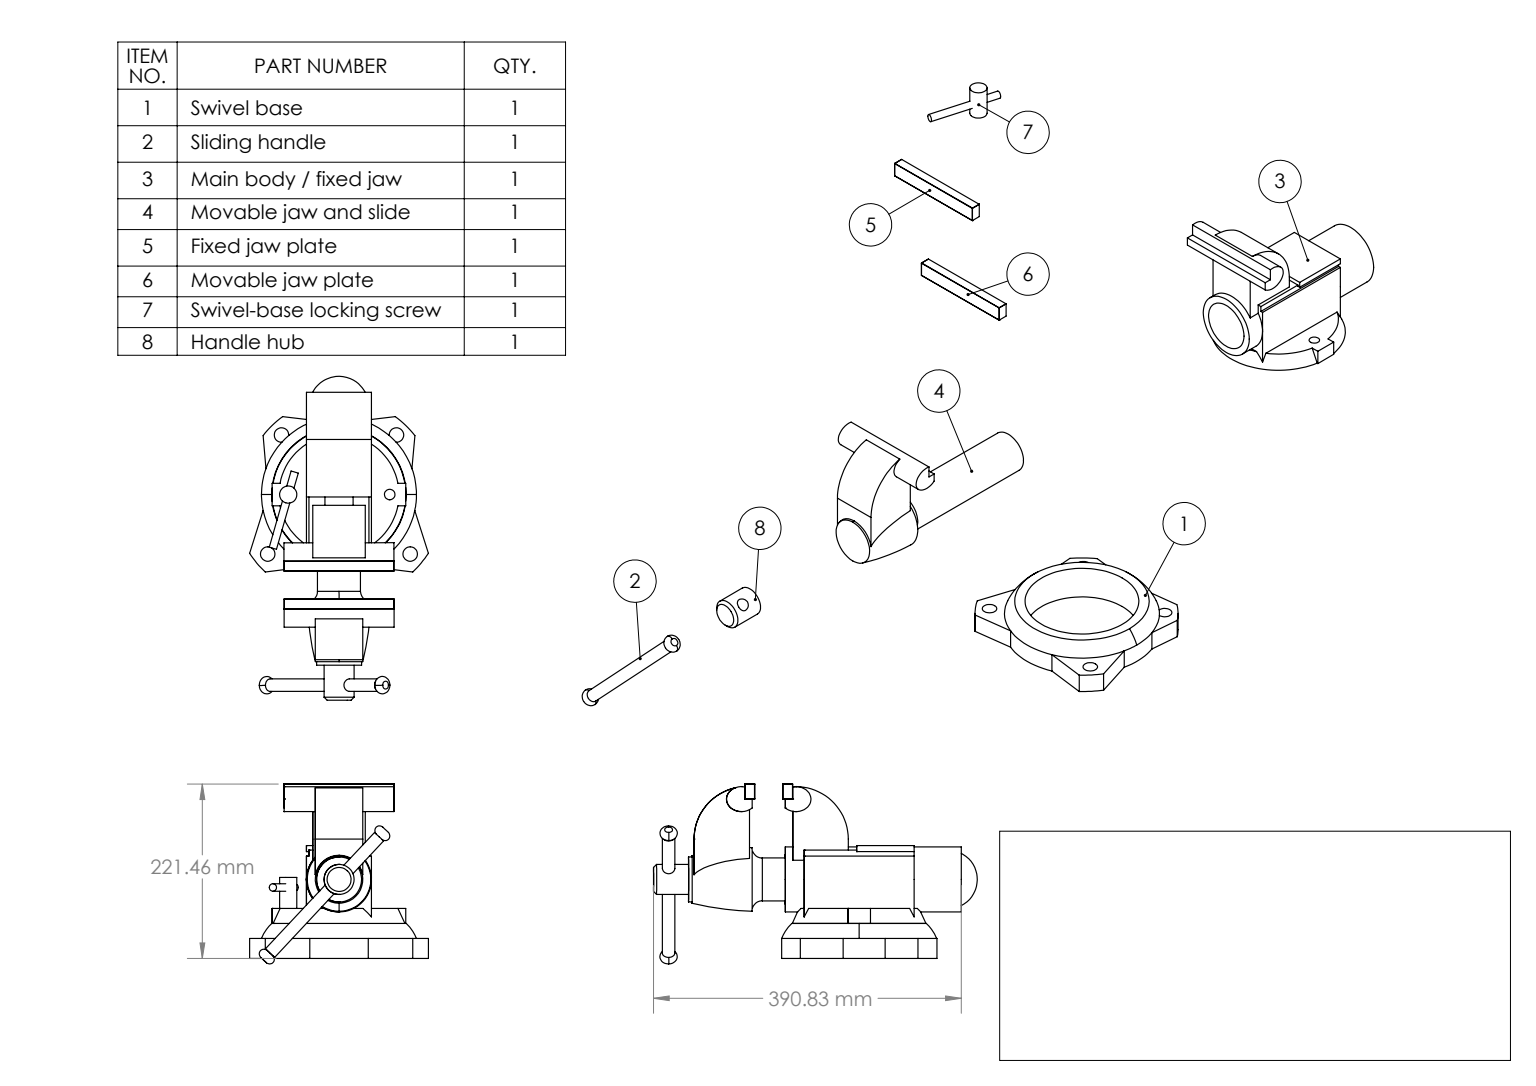
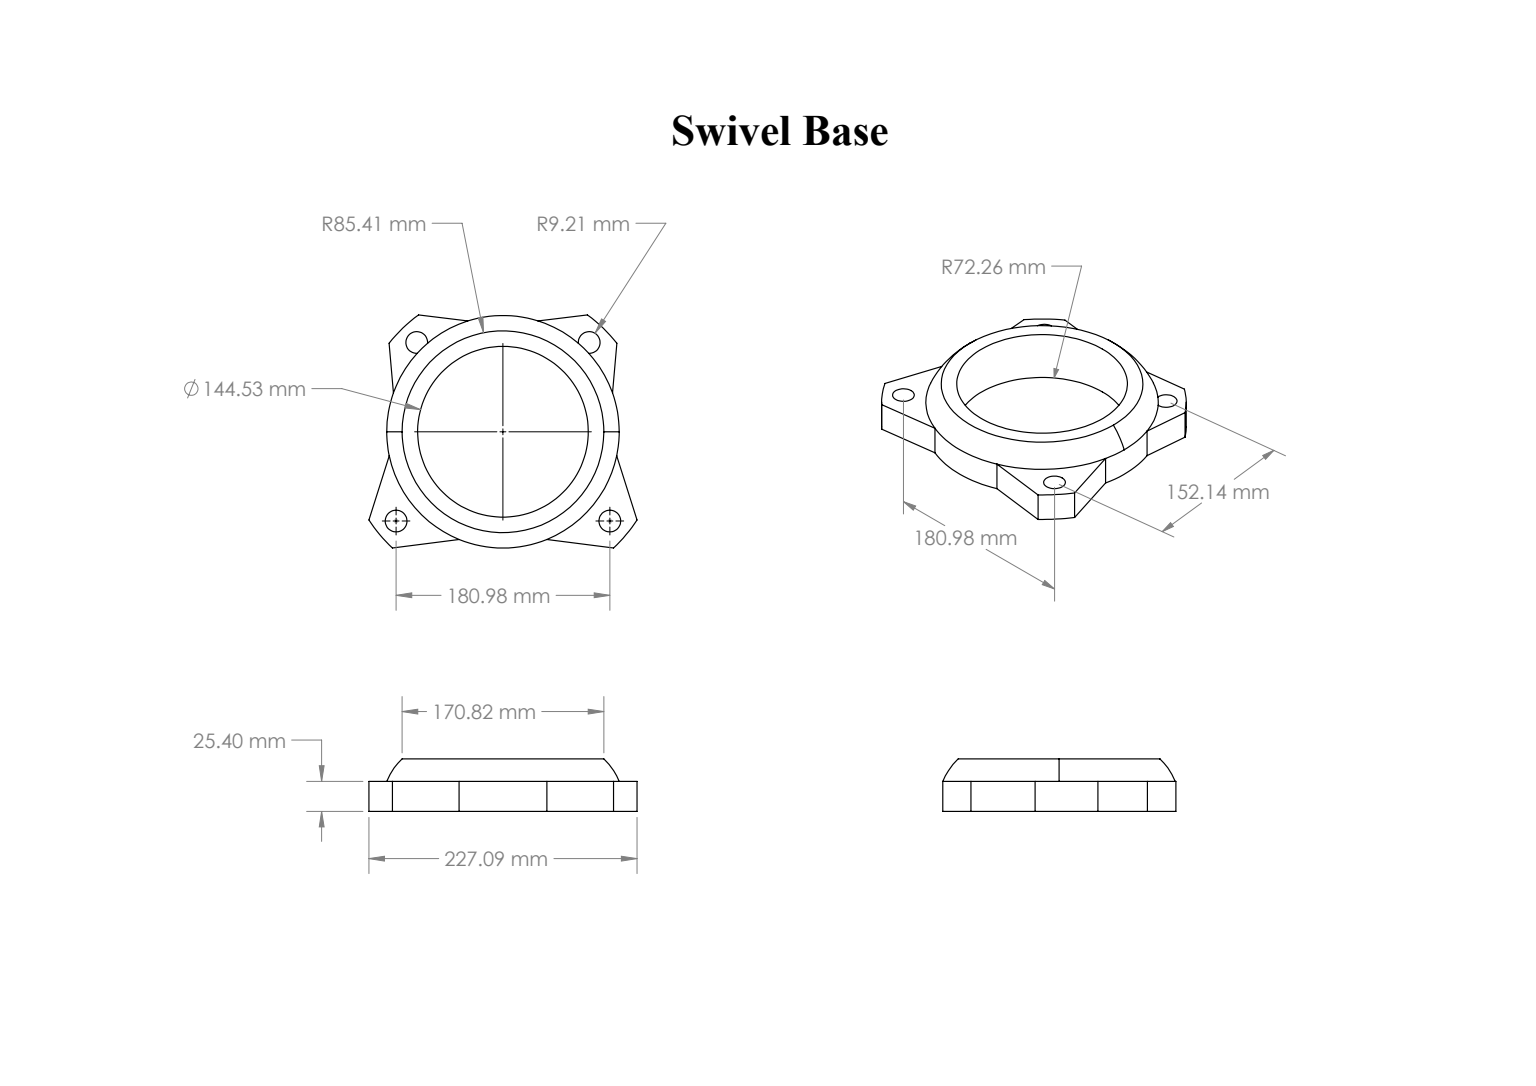
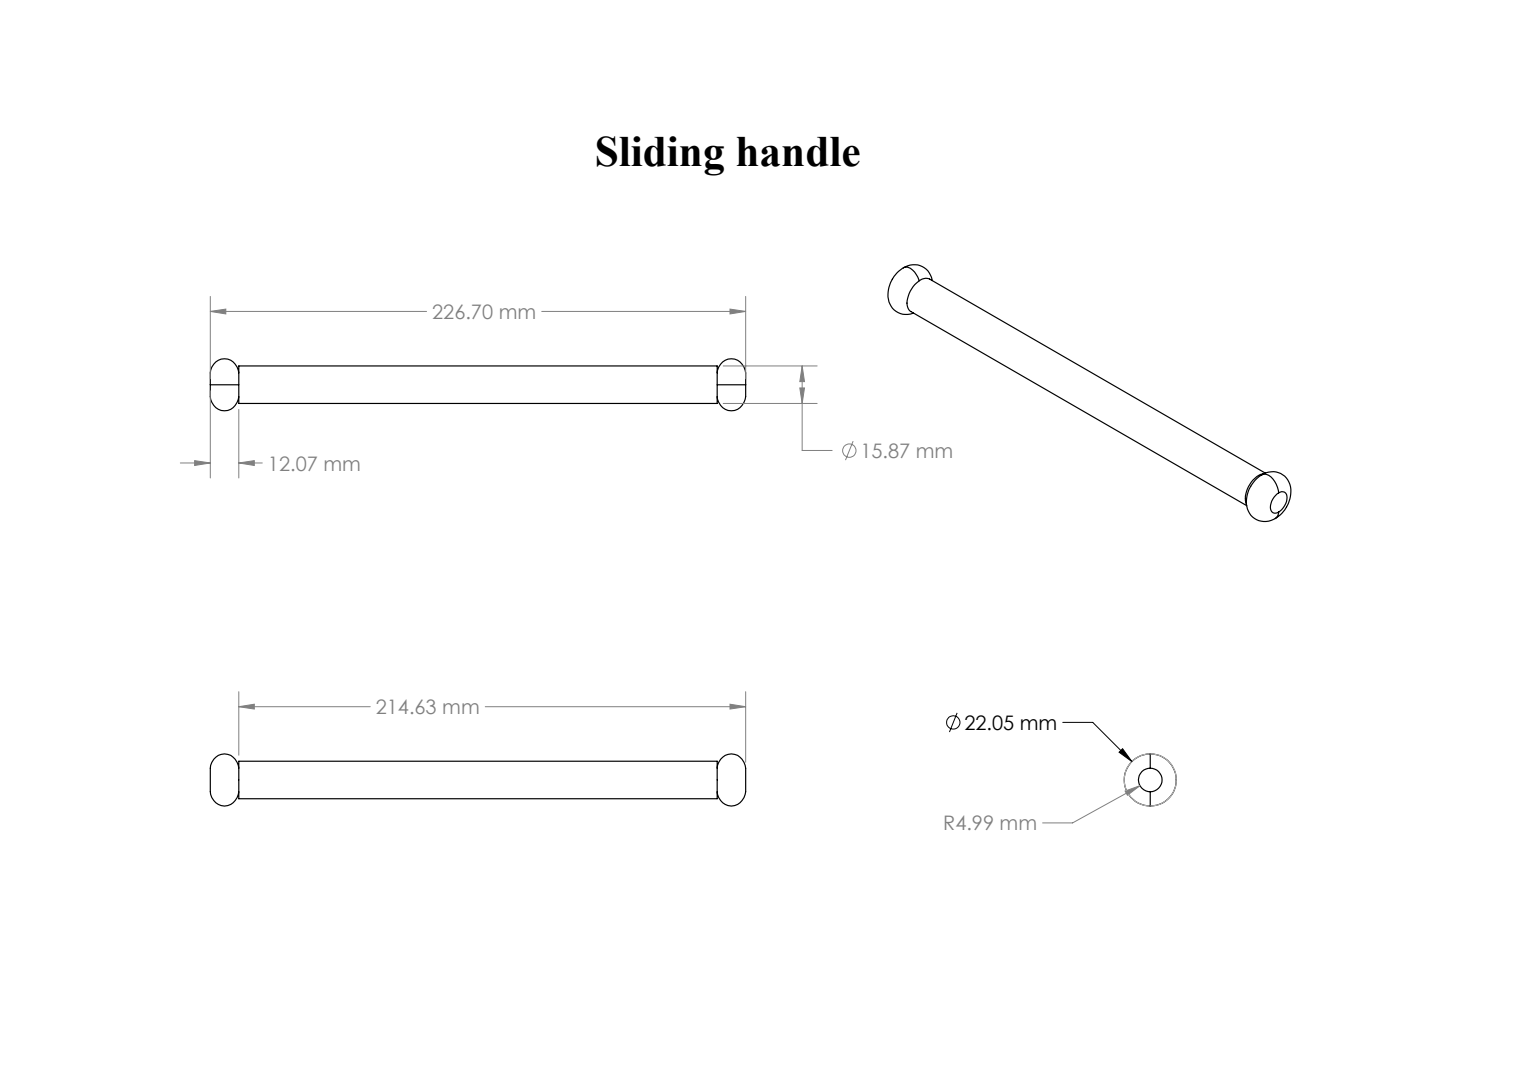
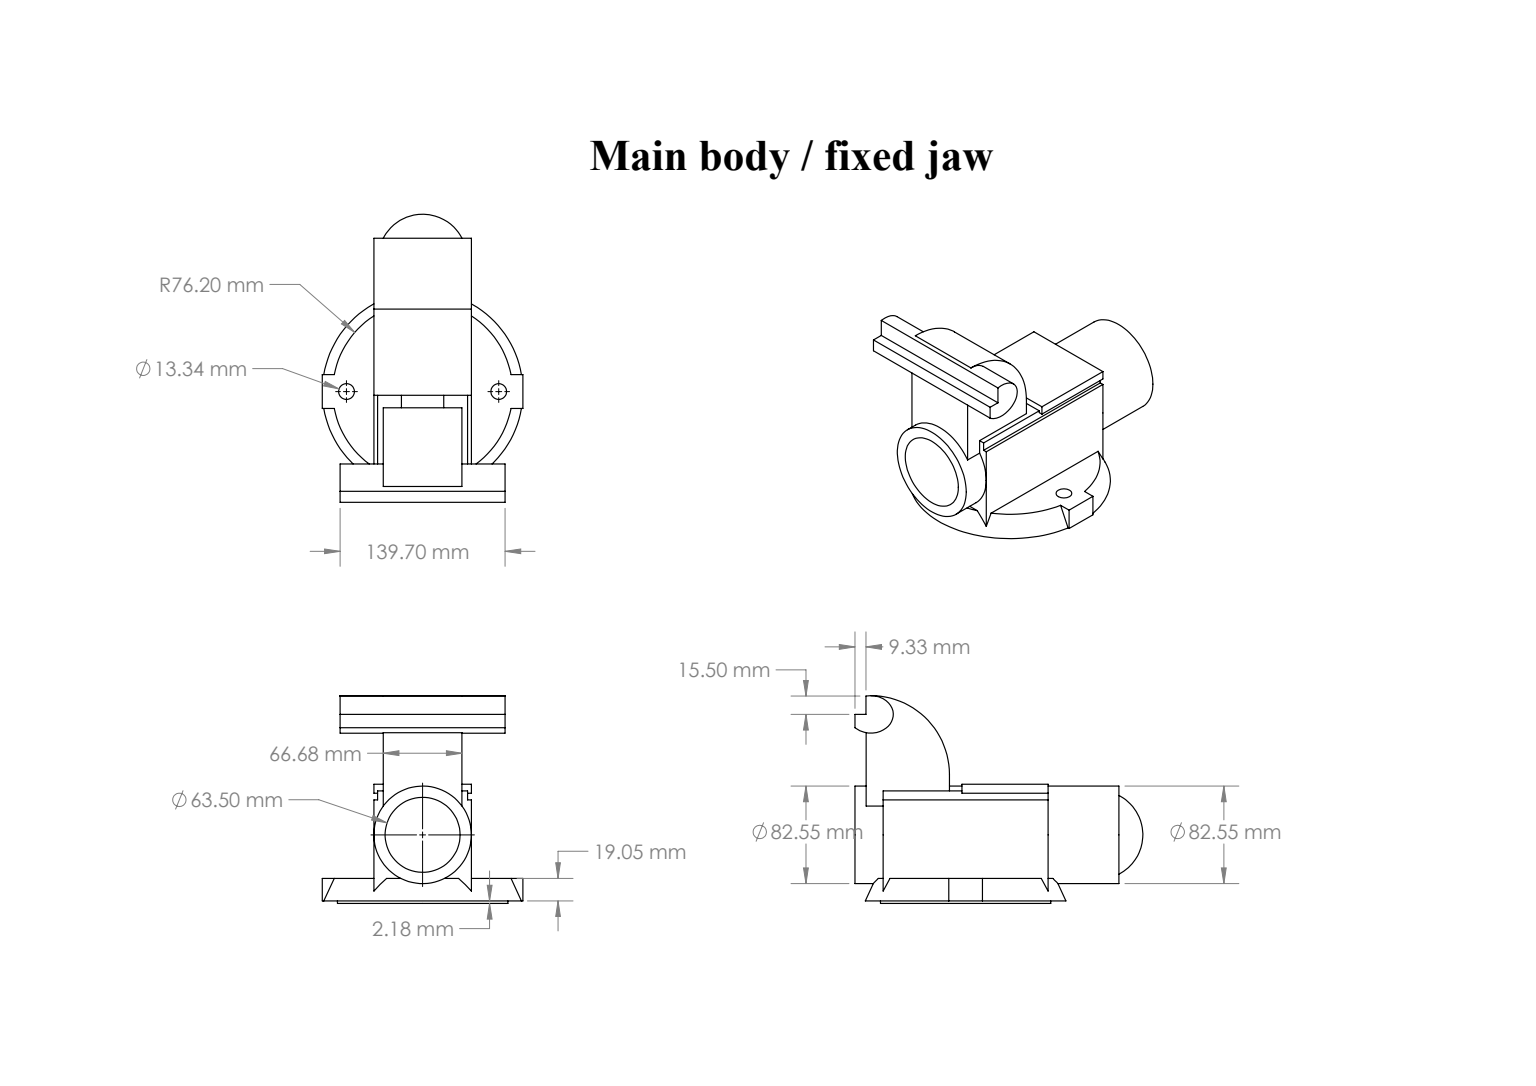
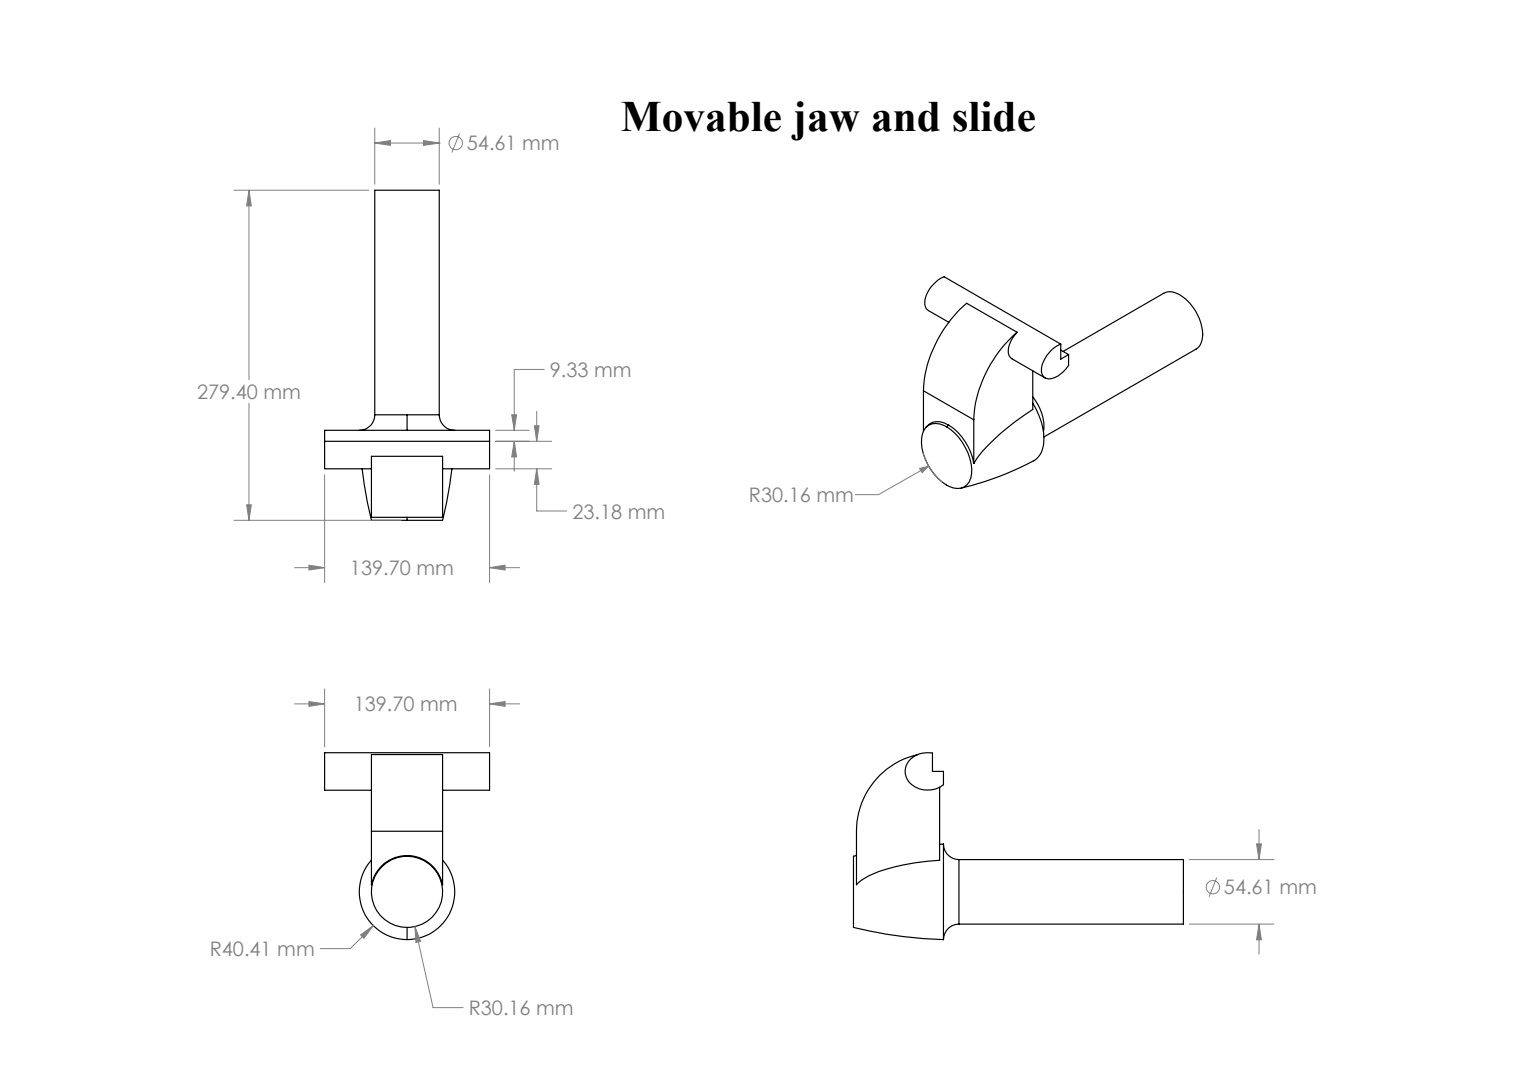
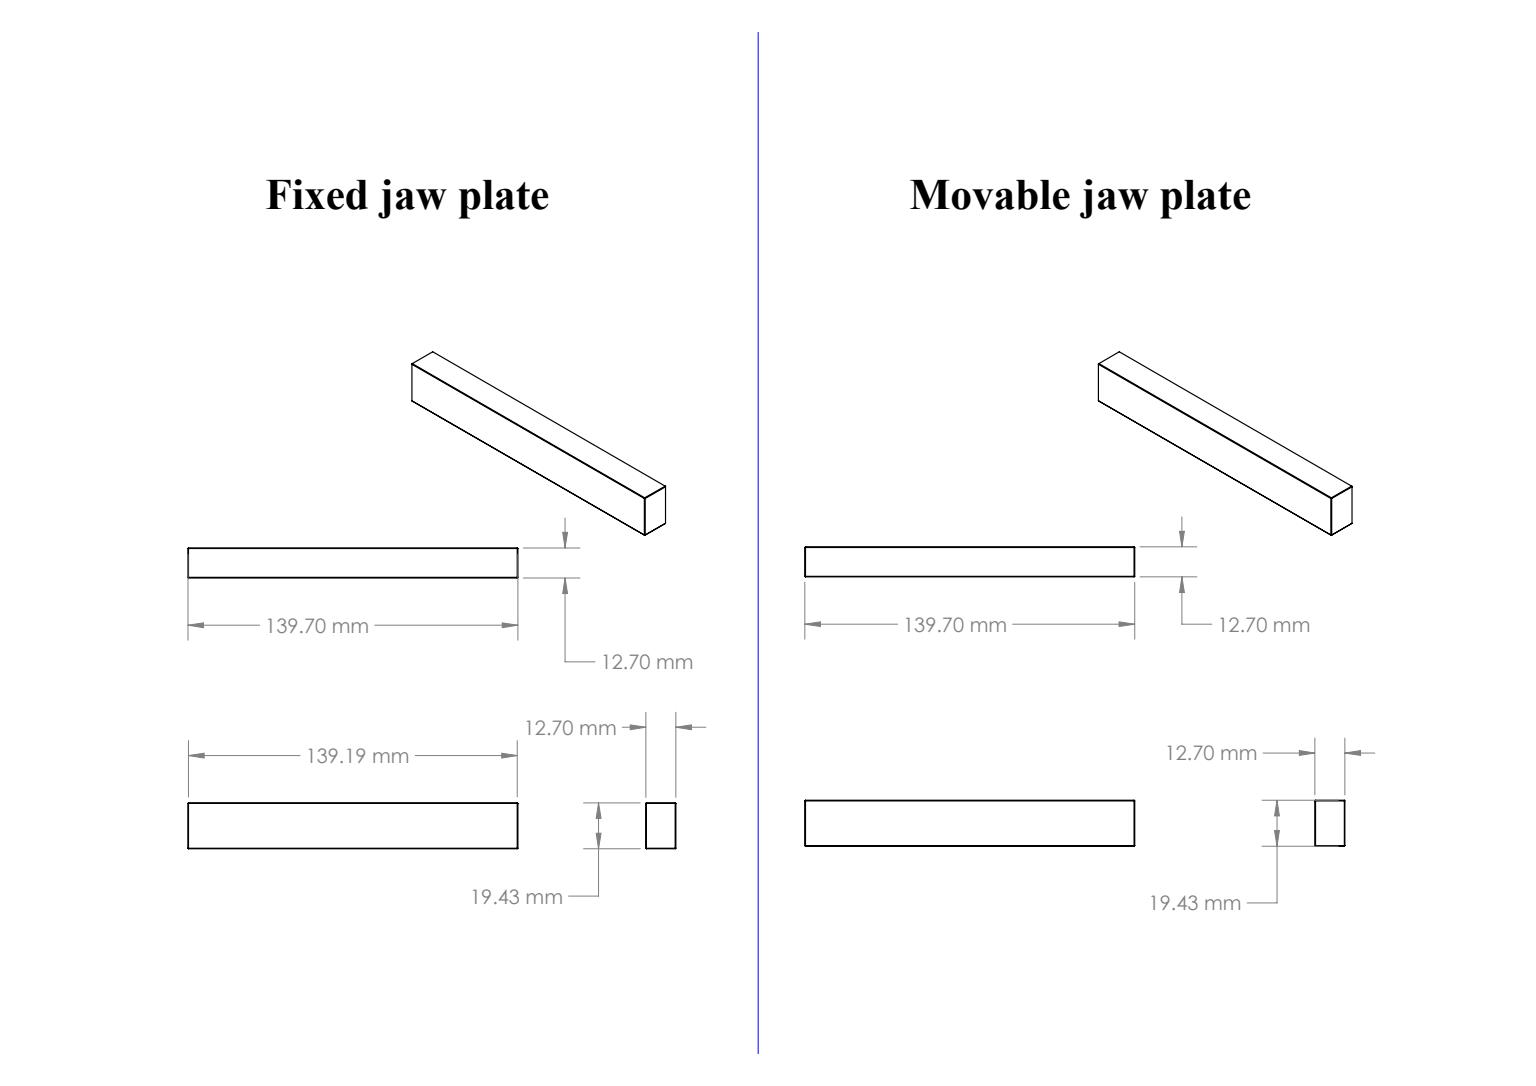
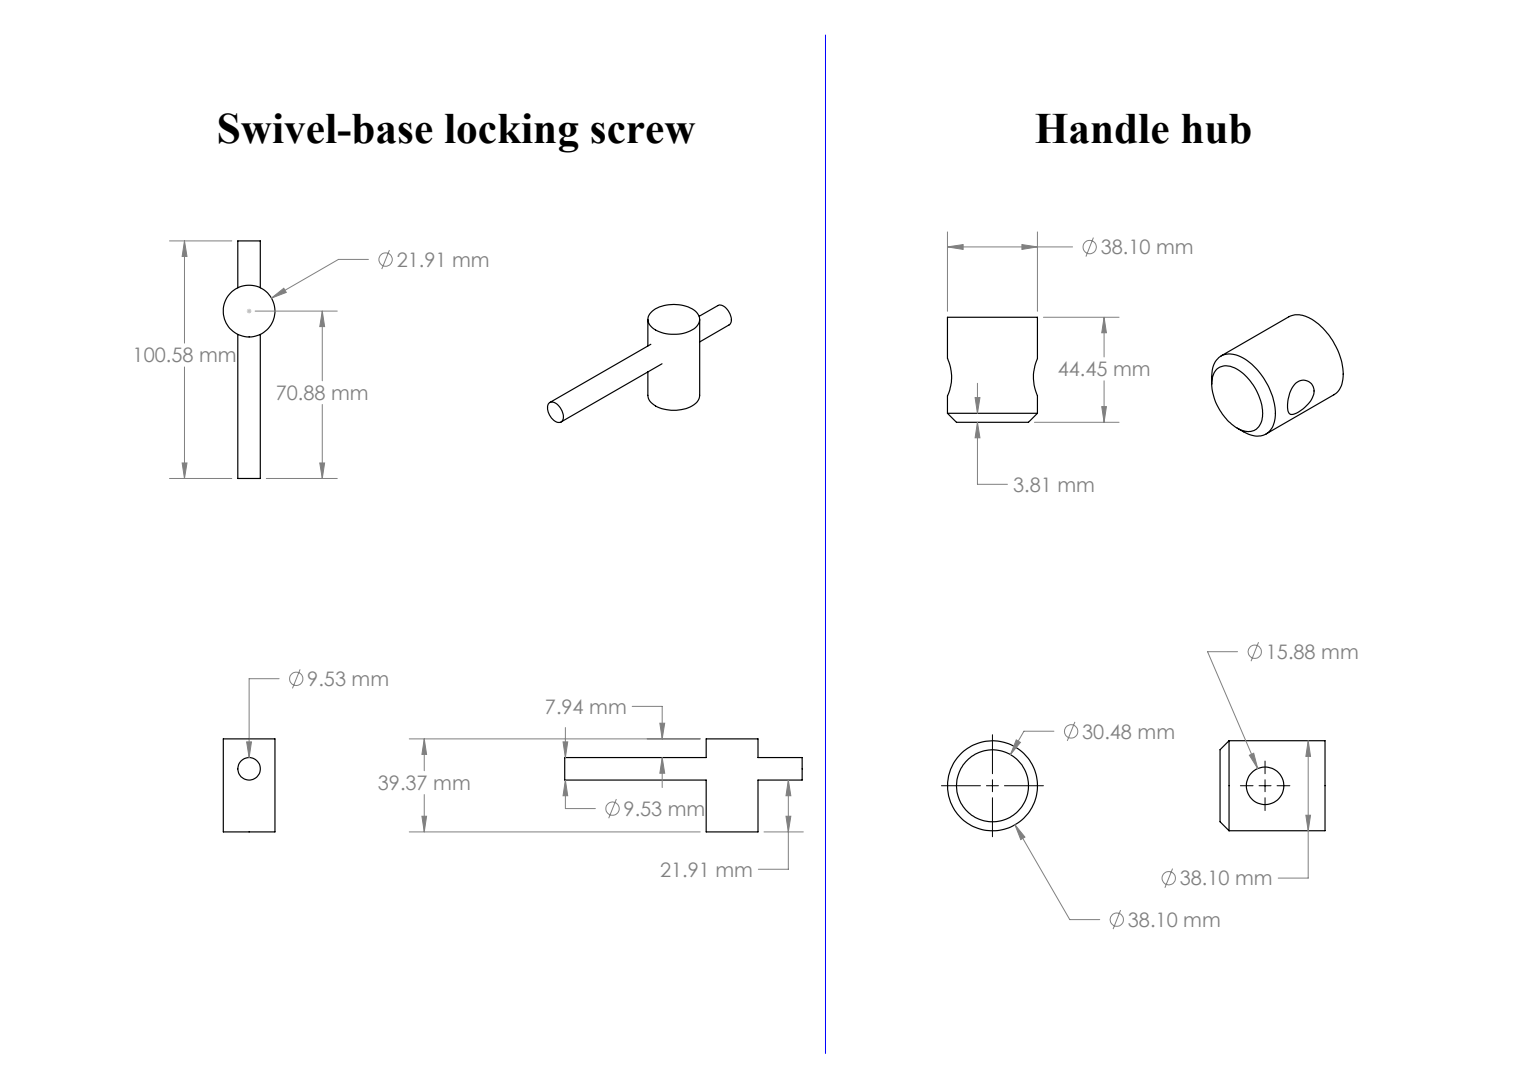
ISO-10303-21;
HEADER;
FILE_DESCRIPTION (('STEP AP203'),
    '1' );
FILE_NAME ('MAS-412',
    '2026-10-07T23:37:23',
    ( '' ),
    ( '' ),
    'SwSTEP 2.0',
    'SolidWorks 2024',
    '' );
FILE_SCHEMA (( 'AUTOMOTIVE_DESIGN' ));
ENDSEC;

DATA;
#1 = EDGE_CURVE ( 'NONE', #6151, #2183, #1599, .T. ) ;
#2 = DIRECTION ( 'NONE',  ( 1.000000000000000000, 0.000000000000000000, 0.000000000000000000 ) ) ;
#3 = CARTESIAN_POINT ( 'NONE',  ( 2.750000000000000444, 8.719000000000002970, 4.313750000000002416 ) ) ;
#4 = CARTESIAN_POINT ( 'NONE',  ( 2.740000000000000213, 8.729000000000002757, 3.333750000000001990 ) ) ;
#5 = ORIENTED_EDGE ( 'NONE', *, *, #5735, .T. ) ;
#6 = CALENDAR_DATE ( 2026, 8, 10 ) ;
#7 = CARTESIAN_POINT ( 'NONE',  ( 2.537500000000000533, 2.500000000000000444, 0.2625000000000008438 ) ) ;
#8 = ADVANCED_FACE ( 'NONE', ( #7344 ), #2858, .F. ) ;
#9 = CARTESIAN_POINT ( 'NONE',  ( -8.751021560936518753E-10, 1.365923996832131609E-16, 5.750408897959578548E-10 ) ) ;
#10 = COORDINATED_UNIVERSAL_TIME_OFFSET ( 0, 0, .AHEAD. ) ;
#11 = CARTESIAN_POINT ( 'NONE',  ( -0.7335700379171464780, 2.500000000182677873, -2.908930215554831999 ) ) ;
#12 = PLANE ( 'NONE',  #8081 ) ;
#13 = ADVANCED_FACE ( 'NONE', ( #7172 ), #6014, .F. ) ;
#14 = AXIS2_PLACEMENT_3D ( 'NONE', #1376, #7034, #673 ) ;
#15 = CYLINDRICAL_SURFACE ( 'NONE', #5940, 2.841000000000000636 ) ;
#16 = CARTESIAN_POINT ( 'NONE',  ( 3.544128228010244186, 1.000000000000000000, 1.972857804739797549 ) ) ;
#17 = ORIENTED_EDGE ( 'NONE', *, *, #5224, .F. ) ;
#18 = LINE ( 'NONE', #3837, #1501 ) ;
#19 = EDGE_CURVE ( 'NONE', #3352, #6547, #5345, .T. ) ;
#20 = CARTESIAN_POINT ( 'NONE',  ( -1.187499999999999778, 4.475358323637860458, 6.462174474937253166 ) ) ;
#21 = APPROVAL_DATE_TIME ( #5612, #98 ) ;
#22 = ORIENTED_EDGE ( 'NONE', *, *, #441, .F. ) ;
#23 = DIRECTION ( 'NONE',  ( 0.000000000000000000, 0.000000000000000000, 1.000000000000000000 ) ) ;
#24 = AXIS2_PLACEMENT_3D ( 'NONE', #1125, #5495, #3538 ) ;
#25 = VECTOR ( 'NONE', #5396, 39.37007874015748143 ) ;
#26 = DIRECTION ( 'NONE',  ( -0.000000000000000000, -1.000000000000000000, -0.000000000000000000 ) ) ;
#27 = LINE ( 'NONE', #5041, #2456 ) ;
#28 = AXIS2_PLACEMENT_3D ( 'NONE', #2617, #7646, #6878 ) ;
#29 = CARTESIAN_POINT ( 'NONE',  ( -2.750000000000000444, 8.601289606299213020, 5.246732086614174229 ) ) ;
#30 = ORIENTED_EDGE ( 'NONE', *, *, #1937, .F. ) ;
#31 = EDGE_LOOP ( 'NONE', ( #4317, #4718, #4653 ) ) ;
#32 = AXIS2_PLACEMENT_3D ( 'NONE', #473, #3002, #4187 ) ;
#33 =( BOUNDED_SURFACE ( )  B_SPLINE_SURFACE ( 3, 3, ( 
 ( #3117, #4870, #7402, #4254 ),
 ( #5609, #6767, #8175, #1152 ),
 ( #198, #3878, #2545, #7053 ),
 ( #4418, #1438, #7009, #3230 ),
 ( #1275, #1924, #4991, #5814 ),
 ( #6924, #3192, #7610, #6392 ) ),
 .UNSPECIFIED., .F., .F., .F. ) 
 B_SPLINE_SURFACE_WITH_KNOTS ( ( 4, 2, 4 ),
 ( 4, 4 ),
 ( 0.000000000000000000, 0.5000000000000000000, 1.000000000000000000 ),
 ( 0.000000000000000000, 1.000000000000000000 ),
 .UNSPECIFIED. ) 
 GEOMETRIC_REPRESENTATION_ITEM ( )  RATIONAL_B_SPLINE_SURFACE ( (
 ( 1.000000000000000000, 0.3333333333333334259, 0.3333333333333334259, 1.000000000000000000),
 ( 1.000000000000000000, 0.3333333333333334259, 0.3333333333333334259, 1.000000000000000000),
 ( 1.000000000000000000, 0.3333333333333334259, 0.3333333333333334259, 1.000000000000000000),
 ( 1.000000000000000000, 0.3333333333333334259, 0.3333333333333334259, 1.000000000000000000),
 ( 1.000000000000000000, 0.3333333333333334259, 0.3333333333333334259, 1.000000000000000000),
 ( 1.000000000000000000, 0.3333333333333334259, 0.3333333333333334259, 1.000000000000000000) ) ) 
 REPRESENTATION_ITEM ( '' )  SURFACE ( )  );
#34 = AXIS2_PLACEMENT_3D ( 'NONE', #7877, #946, #1033 ) ;
#35 = APPROVAL_PERSON_ORGANIZATION ( #57, #5208, #4410 ) ;
#36 = ADVANCED_FACE ( 'NONE', ( #6211 ), #602, .T. ) ;
#37 = CARTESIAN_POINT ( 'NONE',  ( -0.5082965702588324586, 2.405310912759768716, -3.001266468626919259 ) ) ;
#38 = CARTESIAN_POINT ( 'NONE',  ( 0.8670765961576291092, 4.936241069566050577, -5.108749999999999680 ) ) ;
#39 = AXIS2_PLACEMENT_3D ( 'NONE', #7359, #1153, #8008 ) ;
#40 = DIRECTION ( 'NONE',  ( -1.000000000000000000, 0.000000000000000000, 0.000000000000000000 ) ) ;
#41 = VERTEX_POINT ( 'NONE', #2074 ) ;
#42 = ADVANCED_FACE ( 'NONE', ( #1382 ), #6295, .T. ) ;
#43 = DATE_AND_TIME ( #3168, #965 ) ;
#44 = AXIS2_PLACEMENT_3D ( 'NONE', #2089, #4037, #244 ) ;
#45 = CARTESIAN_POINT ( 'NONE',  ( 3.987953385826772390, 3.755224612465394962, 8.262149156879575074 ) ) ;
#46 = CARTESIAN_POINT ( 'NONE',  ( -0.7335374419612978869, 3.792759758930658531, 8.502074107329825381 ) ) ;
#47 = VERTEX_POINT ( 'NONE', #5759 ) ;
#48 = AXIS2_PLACEMENT_3D ( 'NONE', #4004, #7908, #4660 ) ;
#49 = CC_DESIGN_PERSON_AND_ORGANIZATION_ASSIGNMENT ( #5339, #2324, ( #1030 ) ) ;
#50 =( GEOMETRIC_REPRESENTATION_CONTEXT ( 3 ) GLOBAL_UNCERTAINTY_ASSIGNED_CONTEXT ( ( #4134 ) ) GLOBAL_UNIT_ASSIGNED_CONTEXT ( ( #3153, #3070, #7613 ) ) REPRESENTATION_CONTEXT ( 'NONE', 'WORKASPACE' ) );
#51 = FACE_BOUND ( 'NONE', #4197, .T. ) ;
#52 = CARTESIAN_POINT ( 'NONE',  ( 4.462953385826772035, 3.753500037802128375, 8.231249998505111520 ) ) ;
#53 = PLANE ( 'NONE',  #82 ) ;
#54 = ORIENTED_EDGE ( 'NONE', *, *, #6929, .T. ) ;
#55 = APPROVAL_DATE_TIME ( #6339, #5621 ) ;
#56 = CARTESIAN_POINT ( 'NONE',  ( 2.750000000000000444, 8.601278779527561369, 5.246694173228347857 ) ) ;
#57 = PERSON_AND_ORGANIZATION ( #1568, #5834 ) ;
#58 = CARTESIAN_POINT ( 'NONE',  ( -2.740000000000001545, 7.973999999999999311, 4.323750000000001315 ) ) ;
#59 = CARTESIAN_POINT ( 'NONE',  ( 1.625000000000000222, 5.113999999999999879, -2.750000000000000444 ) ) ;
#60 = APPROVAL_PERSON_ORGANIZATION ( #7787, #6874, #5361 ) ;
#61 = ADVANCED_FACE ( 'NONE', ( #5673, #1333, #92, #2030, #51, #5721 ), #132, .F. ) ;
#62 = EDGE_CURVE ( 'NONE', #2284, #7136, #4477, .T. ) ;
#63 = CARTESIAN_POINT ( 'NONE',  ( -3.987046614173229919, 3.872296061808612411, 8.050752829671743882 ) ) ;
#64 = AXIS2_PLACEMENT_3D ( 'NONE', #1983, #3374, #5790 ) ;
#65 = ORIENTED_EDGE ( 'NONE', *, *, #1296, .T. ) ;
#66 = DIRECTION ( 'NONE',  ( 2.664535259084986204E-15, 0.000000000000000000, 1.000000000000000000 ) ) ;
#67 = DIRECTION ( 'NONE',  ( 0.000000000000000000, 0.000000000000000000, 1.000000000000000000 ) ) ;
#68 = CARTESIAN_POINT ( 'NONE',  ( -1.187500000000000000, 4.528589268181947070, 6.350981843454763798 ) ) ;
#69 = DATE_AND_TIME ( #5694, #2477 ) ;
#70 = EDGE_LOOP ( 'NONE', ( #2555, #6227 ) ) ;
#71 = FACE_OUTER_BOUND ( 'NONE', #866, .T. ) ;
#72 = AXIS2_PLACEMENT_3D ( 'NONE', #6327, #85, #2600 ) ;
#73 = CIRCLE ( 'NONE', #872, 1.124999999999999556 ) ;
#74 = CARTESIAN_POINT ( 'NONE',  ( -4.462046614173229564, 3.753500037802127043, 8.231249998505111520 ) ) ;
#75 = VECTOR ( 'NONE', #6916, 39.37007874015748854 ) ;
#76 = PLANE ( 'NONE',  #326 ) ;
#77 = CARTESIAN_POINT ( 'NONE',  ( 0.000000000000000000, 3.950000000000000178, 2.749999999536766992 ) ) ;
#78 = EDGE_CURVE ( 'NONE', #6387, #3627, #5164, .T. ) ;
#79 = EDGE_CURVE ( 'NONE', #5487, #520, #4524, .T. ) ;
#80 = ORIENTED_EDGE ( 'NONE', *, *, #6042, .T. ) ;
#81 = ORIENTED_EDGE ( 'NONE', *, *, #8030, .T. ) ;
#82 = AXIS2_PLACEMENT_3D ( 'NONE', #2571, #5061, #7600 ) ;
#83 = DIRECTION ( 'NONE',  ( 1.000000000000000000, 0.000000000000000000, 0.000000000000000000 ) ) ;
#84 = CARTESIAN_POINT ( 'NONE',  ( -0.001186137648316157355, 2.637500537863615158, -5.108750000000001457 ) ) ;
#85 = DIRECTION ( 'NONE',  ( -1.000000000000000000, 0.000000000000000000, 0.000000000000000000 ) ) ;
#86 = ORIENTED_EDGE ( 'NONE', *, *, #479, .F. ) ;
#87 = CARTESIAN_POINT ( 'NONE',  ( 3.987953385826771946, 3.763524128032369465, 8.293365503768654889 ) ) ;
#88 = DIMENSIONAL_EXPONENTS ( 1.000000000000000000, 0.000000000000000000, 0.000000000000000000, 0.000000000000000000, 0.000000000000000000, 0.000000000000000000, 0.000000000000000000 ) ;
#89 = DIRECTION ( 'NONE',  ( 0.9917930140014037388, -0.000000000000000000, 0.1278538907425633420 ) ) ;
#90 = ORIENTED_EDGE ( 'NONE', *, *, #3285, .F. ) ;
#91 = CARTESIAN_POINT ( 'NONE',  ( 0.000000000000000000, 3.950000000000000178, -5.108750000000001457 ) ) ;
#92 = FACE_BOUND ( 'NONE', #7637, .T. ) ;
#93 = DIRECTION ( 'NONE',  ( 0.7071067811865474617, -0.7071067811865474617, -0.000000000000000000 ) ) ;
#94 =( REPRESENTATION_RELATIONSHIP ('NONE','NONE', #3256, #4813 ) REPRESENTATION_RELATIONSHIP_WITH_TRANSFORMATION ( #6716 )SHAPE_REPRESENTATION_RELATIONSHIP( ) );
#95 = VERTEX_POINT ( 'NONE', #3821 ) ;
#96 = SHAPE_DEFINITION_REPRESENTATION ( #1706, #2780 ) ;
#97 = LINE ( 'NONE', #5064, #3478 ) ;
#98 = APPROVAL ( #5739, 'UNSPECIFIED' ) ;
#99 = CARTESIAN_POINT ( 'NONE',  ( -1.489119986720869093, 2.223645902163796428, 2.750000000000000444 ) ) ;
#100 = PRODUCT_DEFINITION_SHAPE ( 'NONE', 'NONE',  #1914 ) ;
#101 = EDGE_LOOP ( 'NONE', ( #3409, #718, #7066 ) ) ;
#102 = ADVANCED_FACE ( 'NONE', ( #760 ), #2649, .T. ) ;
#103 = CARTESIAN_POINT ( 'NONE',  ( 0.000000000000000000, 1.664000000000000368, 2.693920355039552791E-42 ) ) ;
#104 = CARTESIAN_POINT ( 'NONE',  ( 1.312500000000000444, 8.589000000000002188, 3.161250000147724837 ) ) ;
#105 = CARTESIAN_POINT ( 'NONE',  ( -3.987046614173230363, 4.023873226579398832, 8.413336896757355632 ) ) ;
#106 = ORIENTED_EDGE ( 'NONE', *, *, #5767, .F. ) ;
#107 = CARTESIAN_POINT ( 'NONE',  ( -8.751021560936518753E-10, 1.365923996832131609E-16, 5.750408897959578548E-10 ) ) ;
#108 = CARTESIAN_POINT ( 'NONE',  ( 2.750000000000000444, 8.574153543307087233, 4.323749999999999538 ) ) ;
#109 = B_SPLINE_CURVE_WITH_KNOTS ( 'NONE', 3,
 ( #7082, #3263, #3389, #1429, #5254, #2158, #2655, #2036, #5139, #5854, #6561, #3992, #235, #929, #7685, #3940, #3903, #2080, #4572, #1464, #6222, #3185, #4487, #140, #5807, #5908, #7147, #1492, #3971, #260, #7791, #6408, #825, #7023, #3369, #6543, #3328, #1535, #1412, #2138, #7710, #954, #5832, #214 ),
 .UNSPECIFIED., .F., .F.,
 ( 4, 2, 2, 2, 2, 2, 2, 2, 2, 2, 2, 2, 2, 2, 2, 2, 2, 2, 2, 2, 2, 4 ),
 ( 1.387778780781445676E-17, 0.001568404162335165731, 0.002352606243502761499, 0.003136808324670357917, 0.004705212487005582846, 0.005489414568173214826, 0.006273616649340845071, 0.007842020811676163675, 0.009410424974011483146, 0.01019462705517914375, 0.01097882913634680262, 0.01254723329868211515, 0.01333143537984972891, 0.01411563746101734441, 0.01568404162335264307, 0.01725244578568794346, 0.01882084994802324038, 0.02038925411035854424, 0.02117345619152621525, 0.02195765827269388973, 0.02352606243502923522, 0.02509446659736457724 ),
 .UNSPECIFIED. ) ;
#110 = COORDINATED_UNIVERSAL_TIME_OFFSET ( 0, 0, .AHEAD. ) ;
#111 = ORIENTED_EDGE ( 'NONE', *, *, #1410, .F. ) ;
#112 = CARTESIAN_POINT ( 'NONE',  ( -2.750000000000000444, 8.601278779527561369, 3.691250000000001030 ) ) ;
#113 = EDGE_CURVE ( 'NONE', #6547, #6766, #6910, .T. ) ;
#114 = FACE_OUTER_BOUND ( 'NONE', #4631, .T. ) ;
#115 = DIRECTION ( 'NONE',  ( 0.000000000000000000, -1.000000000000000000, -0.000000000000000000 ) ) ;
#116 = PLANE ( 'NONE',  #837 ) ;
#117 = ORIENTED_EDGE ( 'NONE', *, *, #7488, .F. ) ;
#118 = ADVANCED_FACE ( 'NONE', ( #182 ), #7038, .F. ) ;
#119 = ORIENTED_EDGE ( 'NONE', *, *, #2557, .F. ) ;
#120 = APPROVAL_PERSON_ORGANIZATION ( #3902, #1264, #2035 ) ;
#121 = DIRECTION ( 'NONE',  ( 0.000000000000000000, -1.000000000000000000, 0.000000000000000000 ) ) ;
#122 = CARTESIAN_POINT ( 'NONE',  ( 1.282759084805754402, 3.671339687942380525, -5.108750000000001457 ) ) ;
#123 = CARTESIAN_POINT ( 'NONE',  ( 0.7335700383277801162, 2.500000000390421473, -2.908930215353081383 ) ) ;
#124 = DIRECTION ( 'NONE',  ( 1.000000000000000000, 0.000000000000000000, 0.000000000000000000 ) ) ;
#125 = CARTESIAN_POINT ( 'NONE',  ( 3.987953385826773278, 3.848025092515661161, 8.399350079849197570 ) ) ;
#126 = CARTESIAN_POINT ( 'NONE',  ( 1.624999999336056655, 2.076218727025485933, 2.749999998825987557 ) ) ;
#127 = B_SPLINE_CURVE_WITH_KNOTS ( 'NONE', 3,
 ( #126, #2024, #4520, #1417, #2983, #7595 ),
 .UNSPECIFIED., .F., .F.,
 ( 4, 2, 4 ),
 ( 0.000000000000000000, 0.007631658709671237072, 0.01526331741934247414 ),
 .UNSPECIFIED. ) ;
#128 = ORIENTED_EDGE ( 'NONE', *, *, #4388, .F. ) ;
#129 = ADVANCED_FACE ( 'NONE', ( #841 ), #1421, .F. ) ;
#130 = DIRECTION ( 'NONE',  ( -0.000000000000000000, 1.000000000000000000, -0.000000000000000000 ) ) ;
#131 = DIRECTION ( 'NONE',  ( -0.000000000000000000, -0.000000000000000000, 1.000000000000000000 ) ) ;
#132 = PLANE ( 'NONE',  #3078 ) ;
#133 = DIRECTION ( 'NONE',  ( -0.000000000000000000, -0.000000000000000000, 1.000000000000000000 ) ) ;
#134 = ORIENTED_EDGE ( 'NONE', *, *, #3696, .T. ) ;
#135 = PERSON_AND_ORGANIZATION ( #7862, #8117 ) ;
#136 = CARTESIAN_POINT ( 'NONE',  ( -2.740000000000000657, 7.974000000000001087, 3.323750000000001759 ) ) ;
#137 = COORDINATED_UNIVERSAL_TIME_OFFSET ( 0, 0, .AHEAD. ) ;
#138 = CARTESIAN_POINT ( 'NONE',  ( 3.987953385826772390, 4.262500003889283740, 8.231249998505111520 ) ) ;
#139 = CARTESIAN_POINT ( 'NONE',  ( -1.347488132528783966, 2.365290550993251806, 2.750000000000000444 ) ) ;
#140 = CARTESIAN_POINT ( 'NONE',  ( 0.6817881100752517520, 3.637486043182223128, 8.241141111267671349 ) ) ;
#141 = ORIENTED_EDGE ( 'NONE', *, *, #2782, .T. ) ;
#142 = DIRECTION ( 'NONE',  ( 0.7071067811865475727, 0.7071067811865475727, -0.000000000000000000 ) ) ;
#143 = CARTESIAN_POINT ( 'NONE',  ( 4.476342532109287120, 3.950000015938371689, 8.543749986456024459 ) ) ;
#144 = CC_DESIGN_PERSON_AND_ORGANIZATION_ASSIGNMENT ( #57, #5065, ( #4775 ) ) ;
#145 = CARTESIAN_POINT ( 'NONE',  ( -3.987046614173229475, 3.767882598671322913, 8.305060267424060783 ) ) ;
#146 = EDGE_LOOP ( 'NONE', ( #7906, #6476, #5872, #8033 ) ) ;
#147 = DIRECTION ( 'NONE',  ( 0.000000000000000000, -1.000000000000000000, 0.000000000000000000 ) ) ;
#148 = ORIENTED_EDGE ( 'NONE', *, *, #4983, .T. ) ;
#149 = SHAPE_REPRESENTATION_RELATIONSHIP ( 'NONE' , 'NONE' ,  #2780, #2140 ) ;
#150 = PLANE ( 'NONE',  #5416 ) ;
#151 = DIRECTION ( 'NONE',  ( 0.5773502691896258421, -0.5773502691896258421, -0.5773502691896258421 ) ) ;
#152 = PERSON_AND_ORGANIZATION ( #7862, #8117 ) ;
#153 = ORIENTED_EDGE ( 'NONE', *, *, #632, .T. ) ;
#154 = CC_DESIGN_PERSON_AND_ORGANIZATION_ASSIGNMENT ( #1625, #1590, ( #303 ) ) ;
#155 = LINE ( 'NONE', #7705, #5155 ) ;
#156 = CARTESIAN_POINT ( 'NONE',  ( -2.750000000000000888, 8.574153543307089009, 3.323750000000001315 ) ) ;
#157 = DIRECTION ( 'NONE',  ( 0.000000000000000000, -0.000000000000000000, 1.000000000000000000 ) ) ;
#158 = ORIENTED_EDGE ( 'NONE', *, *, #3778, .F. ) ;
#159 = FACE_OUTER_BOUND ( 'NONE', #7228, .T. ) ;
#160 = CC_DESIGN_APPROVAL ( #4518, ( #1491 ) ) ;
#161 = ORIENTED_EDGE ( 'NONE', *, *, #1, .T. ) ;
#162 = EDGE_CURVE ( 'NONE', #7663, #2678, #722, .T. ) ;
#163 = VECTOR ( 'NONE', #263, 39.37007874015748143 ) ;
#164 = VECTOR ( 'NONE', #2503, 39.37007874015748143 ) ;
#165 = CIRCLE ( 'NONE', #6062, 1.074999999999999289 ) ;
#166 = EDGE_CURVE ( 'NONE', #7244, #3899, #2692, .T. ) ;
#167 = CARTESIAN_POINT ( 'NONE',  ( 3.987953385826771946, 3.848075132174967550, 8.063218304144973203 ) ) ;
#168 = CARTESIAN_POINT ( 'NONE',  ( 0.001186118861278498285, 5.262499470843738258, -5.108750000000001457 ) ) ;
#169 = CARTESIAN_POINT ( 'NONE',  ( 2.740000000000001545, 8.729000000000002757, 3.833750000000001545 ) ) ;
#170 = ORIENTED_EDGE ( 'NONE', *, *, #1035, .F. ) ;
#171 = CARTESIAN_POINT ( 'NONE',  ( 3.987953385826772834, 4.017233591675260840, 8.415903052206910928 ) ) ;
#172 = CARTESIAN_POINT ( 'NONE',  ( -0.7274884641267203023, 3.767418641134390178, 8.485068404623115512 ) ) ;
#173 = AXIS2_PLACEMENT_3D ( 'NONE', #3203, #1935, #2062 ) ;
#174 = ORIENTED_EDGE ( 'NONE', *, *, #2746, .F. ) ;
#175 = PRODUCT_DEFINITION_SHAPE ( 'NONE', 'NONE',  #8189 ) ;
#176 = AXIS2_PLACEMENT_3D ( 'NONE', #828, #121, #3331 ) ;
#177 = EDGE_CURVE ( 'NONE', #1721, #1286, #2037, .T. ) ;
#178 = CARTESIAN_POINT ( 'NONE',  ( -8.751021560936518753E-10, 1.365923996832131609E-16, 5.750408897959578548E-10 ) ) ;
#179 = VECTOR ( 'NONE', #3445, 39.37007874015748143 ) ;
#180 = AXIS2_PLACEMENT_3D ( 'NONE', #661, #26, #4591 ) ;
#181 = VECTOR ( 'NONE', #6775, 39.37007874015748143 ) ;
#182 = FACE_OUTER_BOUND ( 'NONE', #740, .T. ) ;
#183 = CARTESIAN_POINT ( 'NONE',  ( -2.750000000000000444, 8.719000000000002970, 3.833750000000001545 ) ) ;
#184 = ORIENTED_EDGE ( 'NONE', *, *, #6285, .F. ) ;
#185 = APPROVAL_STATUS ( 'not_yet_approved' ) ;
#186 = CARTESIAN_POINT ( 'NONE',  ( 2.750000000000000888, 7.964000000000000412, 3.823750000000002647 ) ) ;
#187 = EDGE_CURVE ( 'NONE', #3123, #5331, #5845, .T. ) ;
#188 = CALENDAR_DATE ( 2026, 8, 10 ) ;
#189 = CARTESIAN_POINT ( 'NONE',  ( -2.078417272059708142E-11, 5.113999999999999879, 2.749999998413802160 ) ) ;
#190 = ADVANCED_FACE ( 'NONE', ( #1297 ), #3855, .T. ) ;
#191 = VECTOR ( 'NONE', #2428, 39.37007874015748854 ) ;
#192 = EDGE_LOOP ( 'NONE', ( #5190, #7911, #4806, #6907 ) ) ;
#193 = CARTESIAN_POINT ( 'NONE',  ( -3.987046614173227699, 4.110686350265323696, 8.118096427185742314 ) ) ;
#194 = CARTESIAN_POINT ( 'NONE',  ( 1.674765980421384803, 1.000000000000000444, -3.533905825348209628 ) ) ;
#195 = AXIS2_PLACEMENT_3D ( 'NONE', #5137, #2034, #1912 ) ;
#196 = CARTESIAN_POINT ( 'NONE',  ( -3.987046614173228143, 3.937513178174820716, 8.427751303491342938 ) ) ;
#197 = ORIENTED_EDGE ( 'NONE', *, *, #7668, .T. ) ;
#198 = CARTESIAN_POINT ( 'NONE',  ( -4.382879947506562068, 3.516000035344543306, 8.231249998505111520 ) ) ;
#199 = AXIS2_PLACEMENT_3D ( 'NONE', #677, #1458, #2606 ) ;
#200 = CC_DESIGN_SECURITY_CLASSIFICATION ( #4775, ( #8192 ) ) ;
#201 = CARTESIAN_POINT ( 'NONE',  ( -2.750000000000000444, 7.541160346212514298, 3.932968645167688404 ) ) ;
#202 = LINE ( 'NONE', #3233, #5994 ) ;
#203 = COORDINATED_UNIVERSAL_TIME_OFFSET ( 0, 0, .AHEAD. ) ;
#204 = ORIENTED_EDGE ( 'NONE', *, *, #4799, .T. ) ;
#205 = AXIS2_PLACEMENT_3D ( 'NONE', #3133, #8065, #544 ) ;
#206 = PLANE ( 'NONE',  #2136 ) ;
#207 = DIRECTION ( 'NONE',  ( 0.000000000000000000, 0.000000000000000000, 1.000000000000000000 ) ) ;
#208 = CARTESIAN_POINT ( 'NONE',  ( -2.750000000000000444, 8.589000000000000412, 2.411250000000000338 ) ) ;
#209 = FACE_OUTER_BOUND ( 'NONE', #5642, .T. ) ;
#210 = DATE_AND_TIME ( #5280, #1629 ) ;
#211 = AXIS2_PLACEMENT_3D ( 'NONE', #382, #6663, #1045 ) ;
#212 = VERTEX_POINT ( 'NONE', #6416 ) ;
#213 = PLANE ( 'NONE',  #3235 ) ;
#214 = CARTESIAN_POINT ( 'NONE',  ( 0.7499999999999993339, 3.950000000000000178, 8.543750000000002842 ) ) ;
#215 = CC_DESIGN_PERSON_AND_ORGANIZATION_ASSIGNMENT ( #7433, #7513, ( #4483 ) ) ;
#216 = EDGE_CURVE ( 'NONE', #5858, #3882, #4440, .T. ) ;
#217 = CARTESIAN_POINT ( 'NONE',  ( 3.987953385826772834, 3.831130030893720395, 8.074194664662527998 ) ) ;
#218 = CARTESIAN_POINT ( 'NONE',  ( 4.383786719160104539, 3.516000035344543750, 8.231249998505111520 ) ) ;
#219 = EDGE_LOOP ( 'NONE', ( #243, #2322, #241, #301 ) ) ;
#220 = CARTESIAN_POINT ( 'NONE',  ( 3.987953385826771946, 3.876943811450185962, 8.413666033243973885 ) ) ;
#221 = AXIS2_PLACEMENT_3D ( 'NONE', #6097, #3140, #4902 ) ;
#222 = EDGE_LOOP ( 'NONE', ( #1976, #4113, #505 ) ) ;
#223 = VECTOR ( 'NONE', #5347, 39.37007874015748854 ) ;
#224 = EDGE_CURVE ( 'NONE', #539, #2109, #923, .T. ) ;
#225 = CARTESIAN_POINT ( 'NONE',  ( 1.624999999336056655, 2.076218727025485933, 2.749999998825987557 ) ) ;
#226 = ADVANCED_FACE ( 'NONE', ( #3542 ), #7853, .F. ) ;
#227 = AXIS2_PLACEMENT_3D ( 'NONE', #112, #741, #2627 ) ;
#228 = EDGE_CURVE ( 'NONE', #1632, #6240, #2956, .T. ) ;
#229 = DIRECTION ( 'NONE',  ( -0.000000000000000000, 1.000000000000000000, 0.000000000000000000 ) ) ;
#230 = DIRECTION ( 'NONE',  ( -0.000000000000000000, -0.000000000000000000, 1.000000000000000000 ) ) ;
#231 = VERTEX_POINT ( 'NONE', #2199 ) ;
#232 = PERSON_AND_ORGANIZATION_ROLE ( 'creator' ) ;
#233 = FACE_OUTER_BOUND ( 'NONE', #3987, .T. ) ;
#234 = COORDINATED_UNIVERSAL_TIME_OFFSET ( 0, 0, .AHEAD. ) ;
#235 = CARTESIAN_POINT ( 'NONE',  ( 0.7188803599037367764, 3.736068989823151387, 8.003234414602296454 ) ) ;
#236 = CARTESIAN_POINT ( 'NONE',  ( 2.537500000000000533, 2.500000000000000444, 0.000000000000000000 ) ) ;
#237 = EDGE_CURVE ( 'NONE', #1328, #4455, #5336, .T. ) ;
#238 = DIRECTION ( 'NONE',  ( 0.000000000000000000, 0.000000000000000000, -1.000000000000000000 ) ) ;
#239 = EDGE_CURVE ( 'NONE', #5017, #7058, #2139, .T. ) ;
#240 = CC_DESIGN_APPROVAL ( #98, ( #3856 ) ) ;
#241 = ORIENTED_EDGE ( 'NONE', *, *, #381, .T. ) ;
#242 = CARTESIAN_POINT ( 'NONE',  ( -3.987046614173229475, 3.771838453700684379, 8.314258565286809954 ) ) ;
#243 = ORIENTED_EDGE ( 'NONE', *, *, #1327, .T. ) ;
#244 = DIRECTION ( 'NONE',  ( 0.000000000000000000, 0.000000000000000000, 1.000000000000000000 ) ) ;
#245 =( LENGTH_UNIT ( ) NAMED_UNIT ( * ) SI_UNIT ( $, .METRE. ) );
#246 = CARTESIAN_POINT ( 'NONE',  ( 1.187500000000000444, 4.987711023622046547, 4.083473622047245399 ) ) ;
#247 = DATE_AND_TIME ( #4620, #3893 ) ;
#248 = ORIENTED_EDGE ( 'NONE', *, *, #2346, .T. ) ;
#249 = EDGE_CURVE ( 'NONE', #3378, #2362, #5077, .T. ) ;
#250 = CARTESIAN_POINT ( 'NONE',  ( 1.625000000000000222, 5.639000000000001123, 0.1249999999999998057 ) ) ;
#251 = CARTESIAN_POINT ( 'NONE',  ( -1.213899175414482112, 4.454554504762766598, -5.108749999999998792 ) ) ;
#252 = EDGE_CURVE ( 'NONE', #2515, #533, #7031, .T. ) ;
#253 = CARTESIAN_POINT ( 'NONE',  ( 2.537500000000000533, 1.664000000000000368, 0.2625000000000008438 ) ) ;
#254 =( NAMED_UNIT ( * ) PLANE_ANGLE_UNIT ( ) SI_UNIT ( $, .RADIAN. ) );
#255 = DIRECTION ( 'NONE',  ( -0.000000000000000000, -0.000000000000000000, 1.000000000000000000 ) ) ;
#256 = ORIENTED_EDGE ( 'NONE', *, *, #6787, .T. ) ;
#257 = COORDINATED_UNIVERSAL_TIME_OFFSET ( 0, 0, .AHEAD. ) ;
#258 = ORIENTED_EDGE ( 'NONE', *, *, #926, .T. ) ;
#259 = CYLINDRICAL_SURFACE ( 'NONE', #8003, 2.841000000000000636 ) ;
#260 = CARTESIAN_POINT ( 'NONE',  ( 0.6955978521287337069, 3.669434091866876635, 8.370402240390431459 ) ) ;
#261 = CARTESIAN_POINT ( 'NONE',  ( 3.562500000000000444, 0.000000000000000000, 2.612499999999998934 ) ) ;
#262 = CC_DESIGN_PERSON_AND_ORGANIZATION_ASSIGNMENT ( #1066, #3017, ( #267 ) ) ;
#263 = DIRECTION ( 'NONE',  ( 1.000000000000000000, 0.000000000000000000, 0.000000000000000000 ) ) ;
#264 = CARTESIAN_POINT ( 'NONE',  ( 2.187663376927555706E-18, 3.950000000000000178, 0.1249999999999999029 ) ) ;
#265 = CARTESIAN_POINT ( 'NONE',  ( 1.312500000000000444, 5.414000000000000590, 0.5414159055118111796 ) ) ;
#266 = VERTEX_POINT ( 'NONE', #3033 ) ;
#267 = SECURITY_CLASSIFICATION ( '', '', #6761 ) ;
#268 = CARTESIAN_POINT ( 'NONE',  ( 0.06610591232966753217, 2.325000000000000622, -3.080208333333334547 ) ) ;
#269 = DIRECTION ( 'NONE',  ( -0.08785522361217638909, 0.000000000000000000, 0.9961332539796342589 ) ) ;
#270 = ORIENTED_EDGE ( 'NONE', *, *, #7587, .T. ) ;
#271 = CC_DESIGN_APPROVAL ( #7758, ( #6576 ) ) ;
#272 = PERSON_AND_ORGANIZATION ( #7862, #8117 ) ;
#273 = CARTESIAN_POINT ( 'NONE',  ( 3.479221556377631263E-16, 1.664000000000000368, -2.841000000000000636 ) ) ;
#274 = CALENDAR_DATE ( 2026, 8, 10 ) ;
#275 = CARTESIAN_POINT ( 'NONE',  ( 3.762484563843161212, 1.281112611882646579, -9.215429355903707278E-16 ) ) ;
#276 = ADVANCED_FACE ( 'NONE', ( #7465 ), #2741, .F. ) ;
#277 = VERTEX_POINT ( 'NONE', #7 ) ;
#278 = DIRECTION ( 'NONE',  ( 0.000000000000000000, -1.000000000000000000, 0.000000000000000000 ) ) ;
#279 = EDGE_CURVE ( 'NONE', #1945, #6623, #5961, .T. ) ;
#280 = CARTESIAN_POINT ( 'NONE',  ( -3.987046614173229475, 4.146499994074616779, 8.243740188835159799 ) ) ;
#281 = ORIENTED_EDGE ( 'NONE', *, *, #1606, .T. ) ;
#282 = DIRECTION ( 'NONE',  ( -1.000000000000000000, 0.000000000000000000, 0.000000000000000000 ) ) ;
#283 = ORIENTED_EDGE ( 'NONE', *, *, #4235, .F. ) ;
#284 = LENGTH_MEASURE_WITH_UNIT ( LENGTH_MEASURE( 0.02539999999999999897 ), #5192 );
#285 = CARTESIAN_POINT ( 'NONE',  ( 2.740000000000001545, 8.729000000000002757, 3.833750000000001545 ) ) ;
#286 = PERSON_AND_ORGANIZATION_ROLE ( 'creator' ) ;
#287 = ORIENTED_EDGE ( 'NONE', *, *, #4323, .T. ) ;
#288 = CARTESIAN_POINT ( 'NONE',  ( -1.178157499656855345, 3.371148463989271260, -5.108749999999998792 ) ) ;
#289 = CARTESIAN_POINT ( 'NONE',  ( 0.6236586488130037020, 2.448156299858527785, 2.959379238582043659 ) ) ;
#290 = CARTESIAN_POINT ( 'NONE',  ( 3.296097360985625002, 1.750000000000000444, 0.5624999982029994516 ) ) ;
#291 =( NAMED_UNIT ( * ) PLANE_ANGLE_UNIT ( ) SI_UNIT ( $, .RADIAN. ) );
#292 = CARTESIAN_POINT ( 'NONE',  ( 1.500000000000000444, 5.414000000000000590, -2.750000000000000444 ) ) ;
#293 = ORIENTED_EDGE ( 'NONE', *, *, #7524, .T. ) ;
#294 = PERSON_AND_ORGANIZATION ( #7862, #8117 ) ;
#295 = VERTEX_POINT ( 'NONE', #6301 ) ;
#296 = EDGE_CURVE ( 'NONE', #3365, #941, #4687, .T. ) ;
#297 = DIRECTION ( 'NONE',  ( 0.000000000000000000, 0.000000000000000000, -1.000000000000000000 ) ) ;
#298 = CARTESIAN_POINT ( 'NONE',  ( 4.067120052493439886, 3.516000035344541974, 7.363250037317452090 ) ) ;
#299 = CARTESIAN_POINT ( 'NONE',  ( -1.172489671586610660, 1.365923996832131609E-16, -3.693357951819909779 ) ) ;
#300 = CARTESIAN_POINT ( 'NONE',  ( 3.987953385826772390, 3.980893307323090546, 8.426027723965566096 ) ) ;
#301 = ORIENTED_EDGE ( 'NONE', *, *, #296, .T. ) ;
#302 = VECTOR ( 'NONE', #7166, 39.37007874015748143 ) ;
#303 = PRODUCT_DEFINITION_FORMATION_WITH_SPECIFIED_SOURCE ( 'ANY', '', #4564, .NOT_KNOWN. ) ;
#304 = CARTESIAN_POINT ( 'NONE',  ( 1.624999999999999556, 2.076218724953421191, -2.749999999536766992 ) ) ;
#305 = DIRECTION ( 'NONE',  ( 0.000000000000000000, -1.000000000000000000, 0.000000000000000000 ) ) ;
#306 = DIRECTION ( 'NONE',  ( 1.000000000000000000, 0.000000000000000000, 0.000000000000000000 ) ) ;
#307 = CARTESIAN_POINT ( 'NONE',  ( 1.074999999999999289, 3.950000000000000178, -4.043750000000001066 ) ) ;
#308 = DATE_AND_TIME ( #5969, #3453 ) ;
#309 = VECTOR ( 'NONE', #4716, 39.37007874015748143 ) ;
#310 = DIRECTION ( 'NONE',  ( 0.000000000000000000, 0.000000000000000000, 1.000000000000000000 ) ) ;
#311 = CALENDAR_DATE ( 2026, 8, 10 ) ;
#312 = CARTESIAN_POINT ( 'NONE',  ( 4.383786719160104539, 3.516000035344543750, 8.231249998505111520 ) ) ;
#313 = CC_DESIGN_PERSON_AND_ORGANIZATION_ASSIGNMENT ( #3468, #6636, ( #6195 ) ) ;
#314 = AXIS2_PLACEMENT_3D ( 'NONE', #4341, #6848, #4999 ) ;
#315 = ORIENTED_EDGE ( 'NONE', *, *, #879, .T. ) ;
#316 = CARTESIAN_POINT ( 'NONE',  ( 0.000000000000000000, 5.541000000000003034, 3.956250000000000266 ) ) ;
#317 = EDGE_CURVE ( 'NONE', #3161, #1533, #4107, .T. ) ;
#318 = CARTESIAN_POINT ( 'NONE',  ( -1.388463899750249738E-31, 3.950000000000000178, -4.043750000000001066 ) ) ;
#319 = EDGE_LOOP ( 'NONE', ( #3487, #7771, #920, #3756, #8180, #5464, #8111, #680 ) ) ;
#320 = CARTESIAN_POINT ( 'NONE',  ( -2.577468385826771957, 5.238734212598424200, 3.956250000000000266 ) ) ;
#321 = ORIENTED_EDGE ( 'NONE', *, *, #4235, .T. ) ;
#322 = PLANE ( 'NONE',  #719 ) ;
#323 = VECTOR ( 'NONE', #3923, 39.37007874015748143 ) ;
#324 = DATE_AND_TIME ( #2127, #631 ) ;
#325 = ORIENTED_EDGE ( 'NONE', *, *, #5751, .T. ) ;
#326 = AXIS2_PLACEMENT_3D ( 'NONE', #29, #2593, #1974 ) ;
#327 = ADVANCED_FACE ( 'NONE', ( #1012 ), #2235, .T. ) ;
#328 = AXIS2_PLACEMENT_3D ( 'NONE', #4120, #1026, #2896 ) ;
#329 = CARTESIAN_POINT ( 'NONE',  ( -1.042238299988425876, 4.752397365051017175, -5.108749999999998792 ) ) ;
#330 = CARTESIAN_POINT ( 'NONE',  ( -4.462046614173229564, 4.146499994074616779, 8.231249998505111520 ) ) ;
#331 = DIRECTION ( 'NONE',  ( -1.000000000000000000, 0.000000000000000000, -0.000000000000000000 ) ) ;
#332 = CARTESIAN_POINT ( 'NONE',  ( -1.312500000000000888, 7.339000000000001300, 3.161250000000001670 ) ) ;
#333 = EDGE_CURVE ( 'NONE', #3882, #4495, #4768, .T. ) ;
#334 = CALENDAR_DATE ( 2026, 8, 10 ) ;
#335 = ORIENTED_EDGE ( 'NONE', *, *, #5247, .F. ) ;
#336 = CARTESIAN_POINT ( 'NONE',  ( -2.740000000000001545, 8.729000000000002757, 3.823750000000002647 ) ) ;
#337 = EDGE_CURVE ( 'NONE', #691, #1844, #2028, .T. ) ;
#338 = CARTESIAN_POINT ( 'NONE',  ( 3.987953385826771946, 3.674333370316265945, 8.231249998505111520 ) ) ;
#339 = ORIENTED_EDGE ( 'NONE', *, *, #1049, .T. ) ;
#340 = LINE ( 'NONE', #2844, #5652 ) ;
#341 = EDGE_LOOP ( 'NONE', ( #1611, #8073, #1909, #7362 ) ) ;
#342 = AXIS2_PLACEMENT_3D ( 'NONE', #4778, #1515, #3551 ) ;
#343 = PLANE ( 'NONE',  #5809 ) ;
#344 = DIRECTION ( 'NONE',  ( -0.000000000000000000, 0.000000000000000000, -1.000000000000000000 ) ) ;
#345 = ADVANCED_FACE ( 'NONE', ( #2970 ), #1788, .F. ) ;
#346 = VECTOR ( 'NONE', #4353, 39.37007874015748143 ) ;
#347 = DIRECTION ( 'NONE',  ( -0.000000000000000000, -0.000000000000000000, 1.000000000000000000 ) ) ;
#348 = AXIS2_PLACEMENT_3D ( 'NONE', #5515, #2418, #7445 ) ;
#349 = EDGE_LOOP ( 'NONE', ( #4385, #197 ) ) ;
#350 = APPLICATION_PROTOCOL_DEFINITION ( 'international standard', 'config_control_design', 1994, #4821 ) ;
#351 = CARTESIAN_POINT ( 'NONE',  ( -2.750000000000000444, 7.964000000000000412, 5.246732086614174229 ) ) ;
#352 = CARTESIAN_POINT ( 'NONE',  ( 0.6863513793485910286, 4.252392623524238857, 8.149781182892043674 ) ) ;
#353 = DIRECTION ( 'NONE',  ( 1.000000000000000000, 0.000000000000000000, -0.000000000000000000 ) ) ;
#354 = AXIS2_PLACEMENT_3D ( 'NONE', #6437, #7092, #3840 ) ;
#355 = ORIENTED_EDGE ( 'NONE', *, *, #2044, .F. ) ;
#356 = CARTESIAN_POINT ( 'NONE',  ( 0.000000000000000000, 1.664000000000000368, 2.693920355039552791E-42 ) ) ;
#357 = CARTESIAN_POINT ( 'NONE',  ( 1.625000000000000222, 2.359134605023787579, -2.598586947582201656 ) ) ;
#358 = LINE ( 'NONE', #2860, #223 ) ;
#359 = ORIENTED_EDGE ( 'NONE', *, *, #4589, .F. ) ;
#360 = APPROVAL_STATUS ( 'not_yet_approved' ) ;
#361 = CC_DESIGN_PERSON_AND_ORGANIZATION_ASSIGNMENT ( #911, #3410, ( #449 ) ) ;
#362 = LINE ( 'NONE', #7823, #7425 ) ;
#363 = FACE_OUTER_BOUND ( 'NONE', #4172, .T. ) ;
#364 = PERSON_AND_ORGANIZATION ( #7862, #8117 ) ;
#365 = EDGE_LOOP ( 'NONE', ( #474, #3997, #3213, #6406 ) ) ;
#366 = ADVANCED_FACE ( 'NONE', ( #3003, #3097 ), #6245, .T. ) ;
#367 = CARTESIAN_POINT ( 'NONE',  ( -0.08777340432027264105, 2.639721318438408293, -5.108750000000001457 ) ) ;
#368 = CARTESIAN_POINT ( 'NONE',  ( 0.7335700383901263555, 2.500000000202698303, 2.908930215426092758 ) ) ;
#369 = CARTESIAN_POINT ( 'NONE',  ( -2.740000000000000657, 7.964000000000000412, 3.333750000000001990 ) ) ;
#370 = CC_DESIGN_APPROVAL ( #1208, ( #7597 ) ) ;
#371 =( NAMED_UNIT ( * ) SI_UNIT ( $, .STERADIAN. ) SOLID_ANGLE_UNIT ( ) );
#372 = CC_DESIGN_PERSON_AND_ORGANIZATION_ASSIGNMENT ( #988, #5472, ( #7291 ) ) ;
#373 = PLANE ( 'NONE',  #3594 ) ;
#374 = APPROVAL_DATE_TIME ( #4673, #3264 ) ;
#375 = ORIENTED_EDGE ( 'NONE', *, *, #2486, .T. ) ;
#376 = CARTESIAN_POINT ( 'NONE',  ( -2.740000000000000657, 7.964000000000000412, 3.333750000000001990 ) ) ;
#377 = CARTESIAN_POINT ( 'NONE',  ( 2.537500000000000533, 2.500000000000000444, -0.4312500000000004663 ) ) ;
#378 = DESIGN_CONTEXT ( 'detailed design', #6135, 'design' ) ;
#379 = EDGE_CURVE ( 'NONE', #7238, #5748, #5501, .T. ) ;
#380 = DIRECTION ( 'NONE',  ( 0.000000000000000000, 0.000000000000000000, -1.000000000000000000 ) ) ;
#381 = EDGE_CURVE ( 'NONE', #3887, #3365, #3166, .T. ) ;
#382 = CARTESIAN_POINT ( 'NONE',  ( -2.750000000000000444, 8.729000000000002757, 3.823750000000002647 ) ) ;
#383 = CARTESIAN_POINT ( 'NONE',  ( 2.375000000000000888, 2.762500000000000178, 6.956249999999999822 ) ) ;
#384 = LINE ( 'NONE', #2356, #6978 ) ;
#385 = ORIENTED_EDGE ( 'NONE', *, *, #7050, .T. ) ;
#386 = CARTESIAN_POINT ( 'NONE',  ( -3.987046614173228587, 4.001800847919961157, 8.041502862977342403 ) ) ;
#387 = CARTESIAN_POINT ( 'NONE',  ( -1.624999999336056877, 2.076218724820237060, -2.750000000000000444 ) ) ;
#388 = EDGE_CURVE ( 'NONE', #6365, #3479, #3288, .T. ) ;
#389 = DIRECTION ( 'NONE',  ( -0.5773502691896258421, -0.5773502691896258421, 0.5773502691896258421 ) ) ;
#390 = ORIENTED_EDGE ( 'NONE', *, *, #1733, .T. ) ;
#391 = APPLICATION_PROTOCOL_DEFINITION ( 'international standard', 'config_control_design', 1994, #2926 ) ;
#392 = DIRECTION ( 'NONE',  ( -0.000000000000000000, -1.000000000000000000, -0.000000000000000000 ) ) ;
#393 = DATE_AND_TIME ( #2365, #6943 ) ;
#394 = CARTESIAN_POINT ( 'NONE',  ( 0.6827599196736721110, 4.260417128052496949, 8.272753927050754186 ) ) ;
#395 = CARTESIAN_POINT ( 'NONE',  ( 0.000000000000000000, 3.950000000000000178, -2.750000000000000444 ) ) ;
#396 = EDGE_LOOP ( 'NONE', ( #4747, #7145, #8060, #3804 ) ) ;
#397 = PLANE ( 'NONE',  #2958 ) ;
#398 = ADVANCED_FACE ( 'NONE', ( #6858 ), #4513, .T. ) ;
#399 = CARTESIAN_POINT ( 'NONE',  ( 1.562500000000000444, 5.639000000000001123, -2.908930215307243383 ) ) ;
#400 = CARTESIAN_POINT ( 'NONE',  ( -8.751021560936518753E-10, 1.365923996832131609E-16, 5.750408897959578548E-10 ) ) ;
#401 = DIRECTION ( 'NONE',  ( -1.000000000000000000, -0.000000000000000000, -0.000000000000000000 ) ) ;
#402 = VERTEX_POINT ( 'NONE', #2400 ) ;
#403 = DATE_AND_TIME ( #6102, #1899 ) ;
#404 = LINE ( 'NONE', #3357, #5288 ) ;
#405 = DIRECTION ( 'NONE',  ( 1.000000000000000000, 0.000000000000000000, -0.000000000000000000 ) ) ;
#406 = DATE_AND_TIME ( #5476, #7356 ) ;
#407 = ORIENTED_EDGE ( 'NONE', *, *, #6294, .T. ) ;
#408 = CARTESIAN_POINT ( 'NONE',  ( 2.750000000000000444, 7.964000000000000412, 3.323750000000001759 ) ) ;
#409 = DIRECTION ( 'NONE',  ( 0.000000000000000000, -0.000000000000000000, 1.000000000000000000 ) ) ;
#410 = CC_DESIGN_DATE_AND_TIME_ASSIGNMENT ( #406, #8078, ( #5099 ) ) ;
#411 = ADVANCED_FACE ( 'NONE', ( #2487 ), #596, .F. ) ;
#412 = DIRECTION ( 'NONE',  ( 1.000000000000000000, -0.000000000000000000, 0.000000000000000000 ) ) ;
#413 = CARTESIAN_POINT ( 'NONE',  ( -2.537500000000000533, 1.664000000000000368, 0.000000000000000000 ) ) ;
#414 = CARTESIAN_POINT ( 'NONE',  ( 2.750000000000000444, 7.521783346456695440, 3.691250000000001030 ) ) ;
#415 = CARTESIAN_POINT ( 'NONE',  ( 3.796513186599488776, 1.365923996832131609E-16, -2.946478861041413211 ) ) ;
#416 = PERSON_AND_ORGANIZATION ( #7862, #8117 ) ;
#417 = VERTEX_POINT ( 'NONE', #2519 ) ;
#418 = DIRECTION ( 'NONE',  ( 0.000000000000000000, 0.000000000000000000, 1.000000000000000000 ) ) ;
#419 = LINE ( 'NONE', #7964, #7254 ) ;
#420 = PRODUCT_RELATED_PRODUCT_CATEGORY ( 'detail', '', ( #2360 ) ) ;
#421 = FACE_BOUND ( 'NONE', #5161, .T. ) ;
#422 = DIRECTION ( 'NONE',  ( 1.000000000000000000, 0.000000000000000000, 0.000000000000000000 ) ) ;
#423 = CARTESIAN_POINT ( 'NONE',  ( 2.750000000000000888, 7.974000000000001087, 3.823750000000002647 ) ) ;
#424 = ORIENTED_EDGE ( 'NONE', *, *, #4346, .T. ) ;
#425 = ADVANCED_FACE ( 'NONE', ( #5050 ), #1169, .F. ) ;
#426 = CARTESIAN_POINT ( 'NONE',  ( -3.987046614173228587, 4.068870000982347968, 8.074194664662202925 ) ) ;
#427 = CARTESIAN_POINT ( 'NONE',  ( -8.751021560936518753E-10, 1.365923996832131609E-16, 5.750408897959578548E-10 ) ) ;
#428 = FACE_OUTER_BOUND ( 'NONE', #3311, .T. ) ;
#429 = ORIENTED_EDGE ( 'NONE', *, *, #735, .T. ) ;
#430 = CALENDAR_DATE ( 2026, 8, 10 ) ;
#431 = CARTESIAN_POINT ( 'NONE',  ( 3.562500000000000444, -3.820994442221351629E-18, 2.975000000000000977 ) ) ;
#432 = AXIS2_PLACEMENT_3D ( 'NONE', #2468, #8085, #6350 ) ;
#433 = APPROVAL_DATE_TIME ( #1745, #6072 ) ;
#434 = CIRCLE ( 'NONE', #4088, 0.3625000012227142521 ) ;
#435 = CC_DESIGN_APPROVAL ( #5120, ( #2483 ) ) ;
#436 = ORIENTED_EDGE ( 'NONE', *, *, #3533, .T. ) ;
#437 = CARTESIAN_POINT ( 'NONE',  ( -3.562500000000000444, 0.000000000000000000, 2.612499999999998934 ) ) ;
#438 = AXIS2_PLACEMENT_3D ( 'NONE', #2910, #5407, #4176 ) ;
#439 = EDGE_LOOP ( 'NONE', ( #407, #3359, #4905, #2556, #2069, #7406 ) ) ;
#440 = CARTESIAN_POINT ( 'NONE',  ( -3.987046614173229031, 4.146499994074616779, 7.838250042232624004 ) ) ;
#441 = EDGE_CURVE ( 'NONE', #5098, #1162, #5449, .T. ) ;
#442 = VERTEX_POINT ( 'NONE', #3979 ) ;
#443 = PERSON_AND_ORGANIZATION ( #7862, #8117 ) ;
#444 = CARTESIAN_POINT ( 'NONE',  ( -1.312500000000000444, 5.414000000000000590, 2.749999994424771721 ) ) ;
#445 = VERTEX_POINT ( 'NONE', #3209 ) ;
#446 = PLANE ( 'NONE',  #5451 ) ;
#447 = VECTOR ( 'NONE', #1168, 39.37007874015748854 ) ;
#448 = VECTOR ( 'NONE', #2131, 39.37007874015748143 ) ;
#449 = PRODUCT_DEFINITION_FORMATION_WITH_SPECIFIED_SOURCE ( 'ANY', '', #6746, .NOT_KNOWN. ) ;
#450 = DIRECTION ( 'NONE',  ( -1.000000000000000000, 0.000000000000000000, -0.000000000000000000 ) ) ;
#451 = CARTESIAN_POINT ( 'NONE',  ( -4.462046614173230452, 4.225666661560478765, 8.231249998505111520 ) ) ;
#452 = AXIS2_PLACEMENT_3D ( 'NONE', #1842, #1114, #5485 ) ;
#453 = CARTESIAN_POINT ( 'NONE',  ( -0.7274884641267199692, 4.132581358865608401, 7.977431595376885731 ) ) ;
#454 = VECTOR ( 'NONE', #2553, 39.37007874015748143 ) ;
#455 = CARTESIAN_POINT ( 'NONE',  ( 2.513411990276540831, 1.000000000000000222, -2.949302488239232023 ) ) ;
#456 =( GEOMETRIC_REPRESENTATION_CONTEXT ( 3 ) GLOBAL_UNCERTAINTY_ASSIGNED_CONTEXT ( ( #7884 ) ) GLOBAL_UNIT_ASSIGNED_CONTEXT ( ( #4708, #254, #948 ) ) REPRESENTATION_CONTEXT ( 'NONE', 'WORKASPACE' ) );
#457 = APPROVAL_DATE_TIME ( #3565, #6638 ) ;
#458 = ORIENTED_EDGE ( 'NONE', *, *, #3599, .F. ) ;
#459 = CARTESIAN_POINT ( 'NONE',  ( -3.762484563843162100, 1.281112611882646579, 4.607714677951853639E-16 ) ) ;
#460 = AXIS2_PLACEMENT_3D ( 'NONE', #1459, #6463, #6417 ) ;
#461 = CARTESIAN_POINT ( 'NONE',  ( 1.625000000000000222, 5.339000000000000412, 0.1249999999999998057 ) ) ;
#462 = DIRECTION ( 'NONE',  ( -0.000000000000000000, -1.000000000000000000, -0.000000000000000000 ) ) ;
#463 = AXIS2_PLACEMENT_3D ( 'NONE', #727, #2610, #4482 ) ;
#464 = CARTESIAN_POINT ( 'NONE',  ( 0.000000000000000000, 3.950000000000000178, 7.131250000000001421 ) ) ;
#465 = ORIENTED_EDGE ( 'NONE', *, *, #3392, .T. ) ;
#466 = CC_DESIGN_DATE_AND_TIME_ASSIGNMENT ( #6860, #1902, ( #5310 ) ) ;
#467 = FACE_OUTER_BOUND ( 'NONE', #758, .T. ) ;
#468 =( BOUNDED_CURVE ( )  B_SPLINE_CURVE ( 3, ( #2510, #4305, #4339, #1282 ),
 .UNSPECIFIED., .F., .F. ) 
 B_SPLINE_CURVE_WITH_KNOTS ( ( 4, 4 ),
 ( 0.000000000000000000, 0.03896959995064044890 ),
 .UNSPECIFIED. ) 
 CURVE ( )  GEOMETRIC_REPRESENTATION_ITEM ( )  RATIONAL_B_SPLINE_CURVE ( ( 0.5120000962196032956, 0.5230192003547537993, 0.5416270346375180456, 0.5678235990678961453 ) ) 
 REPRESENTATION_ITEM ( '' )  );
#469 = ORIENTED_EDGE ( 'NONE', *, *, #1930, .T. ) ;
#470 = AXIS2_PLACEMENT_3D ( 'NONE', #4283, #3546, #7983 ) ;
#471 = DIRECTION ( 'NONE',  ( -0.000000000000000000, 0.000000000000000000, -1.000000000000000000 ) ) ;
#472 = CARTESIAN_POINT ( 'NONE',  ( 2.740000000000001545, 8.729000000000002757, 3.833750000000001545 ) ) ;
#473 = CARTESIAN_POINT ( 'NONE',  ( 0.000000000000000000, 2.500000000000000000, 0.000000000000000000 ) ) ;
#474 = ORIENTED_EDGE ( 'NONE', *, *, #817, .T. ) ;
#475 = DATE_TIME_ROLE ( 'classification_date' ) ;
#476 = EDGE_CURVE ( 'NONE', #1089, #3668, #7630, .T. ) ;
#477 = DIRECTION ( 'NONE',  ( -0.000000000000000000, 1.000000000000000000, 0.000000000000000000 ) ) ;
#478 = ORIENTED_EDGE ( 'NONE', *, *, #3819, .F. ) ;
#479 = EDGE_CURVE ( 'NONE', #1080, #2357, #5711, .T. ) ;
#480 = VECTOR ( 'NONE', #2249, 39.37007874015748143 ) ;
#481 = CARTESIAN_POINT ( 'NONE',  ( -2.861675873811764248, 1.000000000000000222, -2.612744953730403719 ) ) ;
#482 = CIRCLE ( 'NONE', #7583, 1.624999999999999778 ) ;
#483 = CARTESIAN_POINT ( 'NONE',  ( -4.462046614173229564, 4.146499994074616779, 8.231249998505111520 ) ) ;
#484 = DIRECTION ( 'NONE',  ( 0.000000000000000000, 0.000000000000000000, -1.000000000000000000 ) ) ;
#485 = ORIENTED_EDGE ( 'NONE', *, *, #3629, .F. ) ;
#486 = DATE_AND_TIME ( #4784, #1256 ) ;
#487 = ADVANCED_FACE ( 'NONE', ( #7111 ), #3250, .T. ) ;
#488 = DIRECTION ( 'NONE',  ( -0.000000000000000000, 1.000000000000000000, 0.000000000000000000 ) ) ;
#489 = DIRECTION ( 'NONE',  ( -0.000000000000000000, 1.000000000000000000, -0.000000000000000000 ) ) ;
#490 = EDGE_LOOP ( 'NONE', ( #7515, #2757 ) ) ;
#491 = CARTESIAN_POINT ( 'NONE',  ( -1.187500000000000444, 7.964000000000000412, 5.236250000000000071 ) ) ;
#492 = VECTOR ( 'NONE', #6658, 39.37007874015748143 ) ;
#493 = ADVANCED_FACE ( 'NONE', ( #3931 ), #2144, .T. ) ;
#494 = FACE_OUTER_BOUND ( 'NONE', #8010, .T. ) ;
#495 = CARTESIAN_POINT ( 'NONE',  ( 3.687499987877262519, 1.365923996832131609E-16, 3.874999999790589289 ) ) ;
#496 = DIRECTION ( 'NONE',  ( 0.000000000000000000, -1.000000000000000000, 0.000000000000000000 ) ) ;
#497 = FACE_OUTER_BOUND ( 'NONE', #7617, .T. ) ;
#498 = MECHANICAL_CONTEXT ( 'NONE', #4403, 'mechanical' ) ;
#499 = EDGE_LOOP ( 'NONE', ( #1524, #3936, #1377, #8105 ) ) ;
#500 = DIRECTION ( 'NONE',  ( 1.000000000000000000, 0.000000000000000000, 0.000000000000000000 ) ) ;
#501 = EDGE_CURVE ( 'NONE', #5362, #7817, #3859, .T. ) ;
#502 = ORIENTED_EDGE ( 'NONE', *, *, #7720, .T. ) ;
#503 = DIRECTION ( 'NONE',  ( 0.000000000000000000, 0.000000000000000000, -1.000000000000000000 ) ) ;
#504 = CARTESIAN_POINT ( 'NONE',  ( 2.749999999999999556, 7.339000000000003077, 4.175863149606300340 ) ) ;
#505 = ORIENTED_EDGE ( 'NONE', *, *, #5505, .F. ) ;
#506 = DIRECTION ( 'NONE',  ( 1.000000000000000000, 0.000000000000000000, 0.000000000000000000 ) ) ;
#507 = ORIENTED_EDGE ( 'NONE', *, *, #7374, .F. ) ;
#508 = CARTESIAN_POINT ( 'NONE',  ( 3.987953385826772390, 4.118031710298198256, 8.129325114741229541 ) ) ;
#509 = LINE ( 'NONE', #3000, #6718 ) ;
#510 = DIRECTION ( 'NONE',  ( 5.213780441972162403E-17, -8.342048707155459845E-16, -1.000000000000000000 ) ) ;
#511 = CARTESIAN_POINT ( 'NONE',  ( -2.750000000000000444, 7.973999999999999311, 3.823750000000002647 ) ) ;
#512 = ORIENTED_EDGE ( 'NONE', *, *, #2568, .F. ) ;
#513 = COORDINATED_UNIVERSAL_TIME_OFFSET ( 0, 0, .AHEAD. ) ;
#514 = CARTESIAN_POINT ( 'NONE',  ( 0.000000000000000000, 5.339000000000000412, -2.750000000000000444 ) ) ;
#515 = ADVANCED_FACE ( 'NONE', ( #3815 ), #876, .T. ) ;
#516 = PRODUCT_DEFINITION ( 'UNKNOWN', '', #7291, #2103 ) ;
#517 = EDGE_LOOP ( 'NONE', ( #6881, #3552, #6154, #4869 ) ) ;
#518 = DIRECTION ( 'NONE',  ( 1.000000000000000000, 0.000000000000000000, 0.000000000000000000 ) ) ;
#519 = CARTESIAN_POINT ( 'NONE',  ( -4.382879947506562068, 3.516000035344543306, 8.231249998505111520 ) ) ;
#520 = VERTEX_POINT ( 'NONE', #169 ) ;
#521 = PERSON_AND_ORGANIZATION ( #7862, #8117 ) ;
#522 = CARTESIAN_POINT ( 'NONE',  ( -2.875000000000000888, 0.000000000000000000, -3.337500001222715174 ) ) ;
#523 = DIRECTION ( 'NONE',  ( -0.000000000000000000, -0.000000000000000000, 1.000000000000000000 ) ) ;
#524 = PRODUCT_DEFINITION_SHAPE ( 'NONE', 'NONE',  #8188 ) ;
#525 =( REPRESENTATION_RELATIONSHIP ('NONE','NONE', #3256, #6925 ) REPRESENTATION_RELATIONSHIP_WITH_TRANSFORMATION ( #5636 )SHAPE_REPRESENTATION_RELATIONSHIP( ) );
#526 = ADVANCED_FACE ( 'NONE', ( #5172 ), #6456, .T. ) ;
#527 = CARTESIAN_POINT ( 'NONE',  ( -2.861675873811764248, 1.000000000000000222, -2.612744953730403719 ) ) ;
#528 = ORIENTED_EDGE ( 'NONE', *, *, #4439, .F. ) ;
#529 = CARTESIAN_POINT ( 'NONE',  ( -0.7499999999999993339, 3.950000000000000622, 8.543750000000002842 ) ) ;
#530 = LINE ( 'NONE', #1811, #3472 ) ;
#531 = PERSON_AND_ORGANIZATION_ROLE ( 'design_supplier' ) ;
#532 = LOCAL_TIME ( 0, 37, 23.00000000000000000, #1486 ) ;
#533 = VERTEX_POINT ( 'NONE', #5878 ) ;
#534 = CARTESIAN_POINT ( 'NONE',  ( -1.124999999999999556, 3.950000000000000178, 6.956250000000000711 ) ) ;
#535 = ORIENTED_EDGE ( 'NONE', *, *, #479, .T. ) ;
#536 = CARTESIAN_POINT ( 'NONE',  ( -3.296097361031207207, 1.750000000037170489, -0.5624999991015005030 ) ) ;
#537 = LINE ( 'NONE', #4804, #181 ) ;
#538 = EDGE_CURVE ( 'NONE', #2664, #6568, #3093, .T. ) ;
#539 = VERTEX_POINT ( 'NONE', #4472 ) ;
#540 = VERTEX_POINT ( 'NONE', #4559 ) ;
#541 = CARTESIAN_POINT ( 'NONE',  ( 2.740000000000001545, 7.973999999999999311, 3.823750000000002647 ) ) ;
#542 = CARTESIAN_POINT ( 'NONE',  ( 0.04795090551181103306, 5.268934960629921171, -5.098161062992129011 ) ) ;
#543 = DIRECTION ( 'NONE',  ( -0.000000000000000000, 1.000000000000000000, -0.000000000000000000 ) ) ;
#544 = DIRECTION ( 'NONE',  ( 0.000000000000000000, 0.000000000000000000, -1.000000000000000000 ) ) ;
#545 = EDGE_LOOP ( 'NONE', ( #2469, #1170, #5240, #4840 ) ) ;
#546 = DATE_TIME_ROLE ( 'classification_date' ) ;
#547 = CARTESIAN_POINT ( 'NONE',  ( 0.001186118861278498285, 5.262499470843738258, -5.108750000000001457 ) ) ;
#548 = EDGE_CURVE ( 'NONE', #2064, #1699, #5704, .T. ) ;
#549 = ADVANCED_BREP_SHAPE_REPRESENTATION ( '', ( #7369, #7272 ), #3475 ) ;
#550 = ORIENTED_EDGE ( 'NONE', *, *, #7199, .F. ) ;
#551 = CARTESIAN_POINT ( 'NONE',  ( 2.537500000000000533, 4.049999999999999822, 0.4312500000000004663 ) ) ;
#552 = CARTESIAN_POINT ( 'NONE',  ( 2.537499998660271761, 3.737500000000002043, 2.790532913385826763 ) ) ;
#553 = CARTESIAN_POINT ( 'NONE',  ( 1.624999999336056655, 2.076218727025485933, 2.749999998825987557 ) ) ;
#554 = ORIENTED_EDGE ( 'NONE', *, *, #1085, .F. ) ;
#555 = DATE_AND_TIME ( #2496, #7538 ) ;
#556 = DIRECTION ( 'NONE',  ( 0.000000000000000000, 0.000000000000000000, 1.000000000000000000 ) ) ;
#557 = CALENDAR_DATE ( 2026, 8, 10 ) ;
#558 = CC_DESIGN_PERSON_AND_ORGANIZATION_ASSIGNMENT ( #646, #3144, ( #4347 ) ) ;
#559 = AXIS2_PLACEMENT_3D ( 'NONE', #8173, #1922, #3228 ) ;
#560 = VECTOR ( 'NONE', #891, 39.37007874015748143 ) ;
#561 = LOCAL_TIME ( 0, 37, 23.00000000000000000, #513 ) ;
#562 = EDGE_CURVE ( 'NONE', #6048, #2229, #7985, .T. ) ;
#563 = CARTESIAN_POINT ( 'NONE',  ( 2.861675873811764248, 1.000000000000000222, -2.612744953730403719 ) ) ;
#564 = CARTESIAN_POINT ( 'NONE',  ( 2.537500000000000533, 1.664000000000000368, 0.000000000000000000 ) ) ;
#565 = CARTESIAN_POINT ( 'NONE',  ( 0.000000000000000000, 5.153197523761609666, 6.890983900766838310 ) ) ;
#566 = ORIENTED_EDGE ( 'NONE', *, *, #3549, .F. ) ;
#567 = CARTESIAN_POINT ( 'NONE',  ( -0.7335374419612978869, 4.107240241069344044, 7.960425892670178527 ) ) ;
#568 = DIRECTION ( 'NONE',  ( 0.000000000000000000, 0.000000000000000000, 1.000000000000000000 ) ) ;
#569 = DIRECTION ( 'NONE',  ( 1.000000000000000000, 0.000000000000000000, -0.000000000000000000 ) ) ;
#570 = PERSON ( 'NAUO-PER12', 'UNSPECIFIED', 'UNSPECIFIED', ('UNSPECIFIED'), ('UNSPECIFIED'), ('UNSPECIFIED') ) ;
#571 = DATE_AND_TIME ( #6184, #7361 ) ;
#572 = PERSON ( 'NAUO-PER3', 'UNSPECIFIED', 'UNSPECIFIED', ('UNSPECIFIED'), ('UNSPECIFIED'), ('UNSPECIFIED') ) ;
#573 = ORIENTED_EDGE ( 'NONE', *, *, #4497, .F. ) ;
#574 = VECTOR ( 'NONE', #2841, 39.37007874015748143 ) ;
#575 = PLANE ( 'NONE',  #8140 ) ;
#576 = AXIS2_PLACEMENT_3D ( 'NONE', #6538, #4671, #3408 ) ;
#577 = ORIENTED_EDGE ( 'NONE', *, *, #5901, .F. ) ;
#578 = SHAPE_REPRESENTATION ( 'bench vise5-', ( #7272 ), #5419 ) ;
#579 = VECTOR ( 'NONE', #785, 39.37007874015748143 ) ;
#580 = AXIS2_PLACEMENT_3D ( 'NONE', #2554, #7584, #115 ) ;
#581 = CARTESIAN_POINT ( 'NONE',  ( -2.750000000000000444, 8.729000000000002757, 3.823750000000002647 ) ) ;
#582 = CARTESIAN_POINT ( 'NONE',  ( 2.740000000000000657, 7.964000000000000412, 3.813750000000002416 ) ) ;
#583 = CARTESIAN_POINT ( 'NONE',  ( 3.562500000000000444, 1.000000000000000222, 2.975000000000000977 ) ) ;
#584 = VERTEX_POINT ( 'NONE', #7193 ) ;
#585 = CIRCLE ( 'NONE', #4097, 1.624999999999999778 ) ;
#586 = VERTEX_POINT ( 'NONE', #4805 ) ;
#587 = AXIS2_PLACEMENT_3D ( 'NONE', #2371, #4861, #1141 ) ;
#588 =( GEOMETRIC_REPRESENTATION_CONTEXT ( 3 ) GLOBAL_UNCERTAINTY_ASSIGNED_CONTEXT ( ( #4715 ) ) GLOBAL_UNIT_ASSIGNED_CONTEXT ( ( #6311, #3231, #3119 ) ) REPRESENTATION_CONTEXT ( 'NONE', 'WORKASPACE' ) );
#589 = EDGE_CURVE ( 'NONE', #5981, #8092, #4393, .T. ) ;
#590 = ADVANCED_FACE ( 'NONE', ( #4094 ), #4020, .T. ) ;
#591 = AXIS2_PLACEMENT_3D ( 'NONE', #1766, #3689, #7532 ) ;
#592 = CARTESIAN_POINT ( 'NONE',  ( 0.000000000000000000, 3.950000000000000178, -4.308749999765625560 ) ) ;
#593 = LINE ( 'NONE', #4890, #698 ) ;
#594 = CARTESIAN_POINT ( 'NONE',  ( -1.994041535433071610, 4.020147637795276729, -4.886192834645670224 ) ) ;
#595 = APPROVAL_PERSON_ORGANIZATION ( #2156, #5120, #6466 ) ;
#596 = PLANE ( 'NONE',  #1000 ) ;
#597 = ORIENTED_EDGE ( 'NONE', *, *, #4661, .F. ) ;
#598 = PERSON_AND_ORGANIZATION ( #7862, #8117 ) ;
#599 = DIRECTION ( 'NONE',  ( 1.000000000000000000, 0.000000000000000000, -0.000000000000000000 ) ) ;
#600 = SECURITY_CLASSIFICATION ( '', '', #4650 ) ;
#601 = EDGE_CURVE ( 'NONE', #3043, #3479, #4261, .T. ) ;
#602 = PLANE ( 'NONE',  #6628 ) ;
#603 = CARTESIAN_POINT ( 'NONE',  ( 0.000000000000000000, 5.024999999999999467, 3.742515787401575533 ) ) ;
#604 = CARTESIAN_POINT ( 'NONE',  ( 1.500000000000000444, 3.950000000000000178, 2.750000000234376074 ) ) ;
#605 = VERTEX_POINT ( 'NONE', #3537 ) ;
#606 = CIRCLE ( 'NONE', #1393, 1.124999999999999556 ) ;
#607 = MECHANICAL_CONTEXT ( 'NONE', #3567, 'mechanical' ) ;
#608 = CARTESIAN_POINT ( 'NONE',  ( -3.343750000000001776, 1.750000000000000444, 3.383875000000000632 ) ) ;
#609 = APPROVAL_DATE_TIME ( #1215, #2217 ) ;
#610 = DIRECTION ( 'NONE',  ( 0.000000000000000000, 0.000000000000000000, 1.000000000000000000 ) ) ;
#611 = AXIS2_PLACEMENT_3D ( 'NONE', #6702, #6046, #6592 ) ;
#612 = CARTESIAN_POINT ( 'NONE',  ( -3.987046614173229475, 3.753500037802127931, 8.218759808176336890 ) ) ;
#613 = CC_DESIGN_PERSON_AND_ORGANIZATION_ASSIGNMENT ( #4006, #6573, ( #6586 ) ) ;
#614 = CARTESIAN_POINT ( 'NONE',  ( -1.625000000000000222, 5.339000000000000412, -2.750000000000000444 ) ) ;
#615 = VERTEX_POINT ( 'NONE', #2960 ) ;
#616 = CARTESIAN_POINT ( 'NONE',  ( -0.7333924044284368948, 4.107224863919222813, 8.501510692915040579 ) ) ;
#617 = CARTESIAN_POINT ( 'NONE',  ( 0.000000000000000000, 0.000000000000000000, 0.000000000000000000 ) ) ;
#618 = LINE ( 'NONE', #7455, #2288 ) ;
#619 = VECTOR ( 'NONE', #1796, 39.37007874015748143 ) ;
#620 = CALENDAR_DATE ( 2026, 8, 10 ) ;
#621 = AXIS2_PLACEMENT_3D ( 'NONE', #7518, #3053, #3755 ) ;
#622 = ORIENTED_EDGE ( 'NONE', *, *, #4822, .F. ) ;
#623 = CARTESIAN_POINT ( 'NONE',  ( 2.750000000000000888, 7.974000000000001087, 3.333750000000001990 ) ) ;
#624 = DIMENSIONAL_EXPONENTS ( 1.000000000000000000, 0.000000000000000000, 0.000000000000000000, 0.000000000000000000, 0.000000000000000000, 0.000000000000000000, 0.000000000000000000 ) ;
#625 = DIRECTION ( 'NONE',  ( 0.000000000000000000, -0.000000000000000000, 1.000000000000000000 ) ) ;
#626 = CARTESIAN_POINT ( 'NONE',  ( 4.383786719160104539, 4.383999996532199184, 8.231249998505111520 ) ) ;
#627 = DIRECTION ( 'NONE',  ( 1.000000000000000000, 0.000000000000000000, 0.000000000000000000 ) ) ;
#628 = ORIENTED_EDGE ( 'NONE', *, *, #4363, .T. ) ;
#629 = ORIENTED_EDGE ( 'NONE', *, *, #1150, .T. ) ;
#630 =( BOUNDED_CURVE ( )  B_SPLINE_CURVE ( 3, ( #643, #5097, #3106, #4364 ),
 .UNSPECIFIED., .F., .F. ) 
 B_SPLINE_CURVE_WITH_KNOTS ( ( 4, 4 ),
 ( 0.000000000000000000, 0.09428240746600520528 ),
 .UNSPECIFIED. ) 
 CURVE ( )  GEOMETRIC_REPRESENTATION_ITEM ( )  RATIONAL_B_SPLINE_CURVE ( ( 1.000000000000000000, 0.3333333333333330373, 0.3333333333333330373, 1.000000000000000000 ) ) 
 REPRESENTATION_ITEM ( '' )  );
#631 = LOCAL_TIME ( 0, 37, 23.00000000000000000, #2744 ) ;
#632 = EDGE_CURVE ( 'NONE', #2164, #7244, #5794, .T. ) ;
#633 = CARTESIAN_POINT ( 'NONE',  ( -0.3234663987973003807, 2.357191439933449040, -3.048510081330109589 ) ) ;
#634 = CARTESIAN_POINT ( 'NONE',  ( 1.042238314306938918, 3.147602674133755496, -5.108750000000002345 ) ) ;
#635 = DIRECTION ( 'NONE',  ( 0.000000000000000000, 1.000000000000000000, 0.000000000000000000 ) ) ;
#636 = ORIENTED_EDGE ( 'NONE', *, *, #2488, .F. ) ;
#637 = APPROVAL_STATUS ( 'not_yet_approved' ) ;
#638 = CARTESIAN_POINT ( 'NONE',  ( -1.172489671586611548, 1.365923996832131609E-16, -3.693357951819908891 ) ) ;
#639 = CARTESIAN_POINT ( 'NONE',  ( -0.7431911064911159714, 3.848678615087431698, 8.527048809074745606 ) ) ;
#640 = ORIENTED_EDGE ( 'NONE', *, *, #3833, .F. ) ;
#641 = CYLINDRICAL_SURFACE ( 'NONE', #6649, 5.349138356872925826 ) ;
#642 = DIRECTION ( 'NONE',  ( 0.000000000000000000, 1.000000000000000000, -0.000000000000000000 ) ) ;
#643 = CARTESIAN_POINT ( 'NONE',  ( 0.000000000000000000, 2.762500000000000178, 6.956250000000000711 ) ) ;
#644 = PLANE ( 'NONE',  #5989 ) ;
#645 = ORIENTED_EDGE ( 'NONE', *, *, #6517, .F. ) ;
#646 = PERSON_AND_ORGANIZATION ( #7862, #8117 ) ;
#647 = FACE_OUTER_BOUND ( 'NONE', #2462, .T. ) ;
#648 = ITEM_DEFINED_TRANSFORMATION ( 'NONE', 'NONE', #7840,  #5158 ) ;
#649 = DIRECTION ( 'NONE',  ( 0.000000000000000000, 0.000000000000000000, 1.000000000000000000 ) ) ;
#650 = CARTESIAN_POINT ( 'NONE',  ( -3.987046614173228587, 3.781968321577594772, 8.129325114742682601 ) ) ;
#651 = CARTESIAN_POINT ( 'NONE',  ( 2.750000000000000888, 8.719000000000001194, 3.823750000000002647 ) ) ;
#652 = PLANE ( 'NONE',  #1485 ) ;
#653 = EDGE_LOOP ( 'NONE', ( #6266, #7461, #5848, #1274 ) ) ;
#654 = CARTESIAN_POINT ( 'NONE',  ( -2.750000000000000444, 7.521783346469146814, 3.956249999992520916 ) ) ;
#655 = CARTESIAN_POINT ( 'NONE',  ( 1.624999999999999778, 3.950000000000000178, 3.691250000234376216 ) ) ;
#656 = CALENDAR_DATE ( 2026, 8, 10 ) ;
#657 = EDGE_LOOP ( 'NONE', ( #1299, #2971, #6391, #5149 ) ) ;
#658 = DIRECTION ( 'NONE',  ( 0.7071067811865474617, 0.000000000000000000, -0.7071067811865474617 ) ) ;
#659 = ADVANCED_BREP_SHAPE_REPRESENTATION ( '', ( #4597, #7272 ), #3062 ) ;
#660 = ORGANIZATION ( 'NAUO-ORG10', 'UNSPECIFIED', 'UNSPECIFIED' ) ;
#661 = CARTESIAN_POINT ( 'NONE',  ( -2.875000000000000888, -3.820994292482255198E-18, -2.975000000000000977 ) ) ;
#662 = CC_DESIGN_APPROVAL ( #8075, ( #267 ) ) ;
#663 = DIRECTION ( 'NONE',  ( 0.000000000000000000, -0.000000000000000000, 1.000000000000000000 ) ) ;
#664 = ORIENTED_EDGE ( 'NONE', *, *, #7776, .T. ) ;
#665 = ORIENTED_EDGE ( 'NONE', *, *, #7096, .T. ) ;
#666 = APPROVAL ( #7602, 'UNSPECIFIED' ) ;
#667 = DIRECTION ( 'NONE',  ( 0.000000000000000000, 1.000000000000000000, -0.000000000000000000 ) ) ;
#668 = CARTESIAN_POINT ( 'NONE',  ( 1.168432146579409636, 4.548236705813060610, -5.108749999999999680 ) ) ;
#669 = DIRECTION ( 'NONE',  ( 1.000000000000000000, 0.000000000000000000, -0.000000000000000000 ) ) ;
#670 = EDGE_CURVE ( 'NONE', #1901, #3103, #606, .T. ) ;
#671 = ORIENTED_EDGE ( 'NONE', *, *, #7837, .T. ) ;
#672 = SECURITY_CLASSIFICATION_LEVEL ( 'unclassified' ) ;
#673 = DIRECTION ( 'NONE',  ( 1.000000000000000000, 0.000000000000000000, 0.000000000000000000 ) ) ;
#674 = VERTEX_POINT ( 'NONE', #1698 ) ;
#675 = EDGE_CURVE ( 'NONE', #2688, #7591, #5453, .T. ) ;
#676 = CARTESIAN_POINT ( 'NONE',  ( -2.750000000000000444, 7.964000000000001300, 3.323750000000001759 ) ) ;
#677 = CARTESIAN_POINT ( 'NONE',  ( -1.388463899750249738E-31, 3.950000000000000178, -4.043750000000001066 ) ) ;
#678 = CARTESIAN_POINT ( 'NONE',  ( 1.187500000000000222, 8.351123808915705382, 5.236250000000000959 ) ) ;
#679 = LINE ( 'NONE', #3142, #2459 ) ;
#680 = ORIENTED_EDGE ( 'NONE', *, *, #1941, .T. ) ;
#681 = DATE_TIME_ROLE ( 'creation_date' ) ;
#682 = DIRECTION ( 'NONE',  ( -1.000000000000000000, 0.000000000000000000, 0.000000000000000000 ) ) ;
#683 = DATE_TIME_ROLE ( 'classification_date' ) ;
#684 = CARTESIAN_POINT ( 'NONE',  ( 2.740000000000001545, 7.964000000000000412, 4.313750000000002416 ) ) ;
#685 = DIRECTION ( 'NONE',  ( -1.000000000000000000, -0.000000000000000000, -0.000000000000000000 ) ) ;
#686 = ADVANCED_FACE ( 'NONE', ( #1004 ), #2801, .T. ) ;
#687 = CARTESIAN_POINT ( 'NONE',  ( -3.987046614173228587, 3.848025092515166001, 8.063149917161112512 ) ) ;
#688 = EDGE_CURVE ( 'NONE', #7723, #4873, #1653, .T. ) ;
#689 = CARTESIAN_POINT ( 'NONE',  ( -2.750000000000000444, 7.973999999999999311, 3.823750000000002647 ) ) ;
#690 = CARTESIAN_POINT ( 'NONE',  ( 3.362500000000000711, 1.750000000000000444, 0.000000000000000000 ) ) ;
#691 = VERTEX_POINT ( 'NONE', #387 ) ;
#692 = DIRECTION ( 'NONE',  ( -1.000000000000000000, 0.000000000000000000, 0.000000000000000000 ) ) ;
#693 = CYLINDRICAL_SURFACE ( 'NONE', #8106, 0.3625000000000019318 ) ;
#694 = CARTESIAN_POINT ( 'NONE',  ( 0.000000000000000000, 2.359000000000000874, 3.956250000000000266 ) ) ;
#695 = APPLICATION_PROTOCOL_DEFINITION ( 'international standard', 'config_control_design', 1994, #7847 ) ;
#696 = ORIENTED_EDGE ( 'NONE', *, *, #6452, .T. ) ;
#697 = DIRECTION ( 'NONE',  ( 1.000000000000000000, 0.000000000000000000, 0.000000000000000000 ) ) ;
#698 = VECTOR ( 'NONE', #4968, 39.37007874015748143 ) ;
#699 = ADVANCED_FACE ( 'NONE', ( #7242 ), #3421, .T. ) ;
#700 = APPROVAL_PERSON_ORGANIZATION ( #4906, #666, #8123 ) ;
#701 = VECTOR ( 'NONE', #8015, 39.37007874015748143 ) ;
#702 = VECTOR ( 'NONE', #8171, 39.37007874015748143 ) ;
#703 = FACE_OUTER_BOUND ( 'NONE', #499, .T. ) ;
#704 = DIRECTION ( 'NONE',  ( -0.7071067811865474617, 0.000000000000000000, 0.7071067811865474617 ) ) ;
#705 = CC_DESIGN_APPROVAL ( #6376, ( #6195 ) ) ;
#706 = ORIENTED_EDGE ( 'NONE', *, *, #79, .T. ) ;
#707 = LINE ( 'NONE', #751, #5136 ) ;
#708 = ORIENTED_EDGE ( 'NONE', *, *, #1597, .F. ) ;
#709 = VECTOR ( 'NONE', #7101, 39.37007874015748143 ) ;
#710 = CIRCLE ( 'NONE', #5820, 0.2625000000000008438 ) ;
#711 = CARTESIAN_POINT ( 'NONE',  ( 3.987953385826773278, 3.768538842735476457, 8.155839089539284714 ) ) ;
#712 = CC_DESIGN_PERSON_AND_ORGANIZATION_ASSIGNMENT ( #7360, #1154, ( #6576 ) ) ;
#713 = CARTESIAN_POINT ( 'NONE',  ( 0.3381868679734887362, 2.681086572149180558, -5.108749999999998792 ) ) ;
#714 = DIRECTION ( 'NONE',  ( -0.000000000000000000, -1.000000000000000000, -0.000000000000000000 ) ) ;
#715 = ORIENTED_EDGE ( 'NONE', *, *, #4776, .F. ) ;
#716 = CARTESIAN_POINT ( 'NONE',  ( 2.537500000000000533, 2.500000000000000444, 0.2625000000000008438 ) ) ;
#717 = CIRCLE ( 'NONE', #5284, 1.074999999999999289 ) ;
#718 = ORIENTED_EDGE ( 'NONE', *, *, #4210, .T. ) ;
#719 = AXIS2_PLACEMENT_3D ( 'NONE', #901, #7260, #5863 ) ;
#720 =( GEOMETRIC_REPRESENTATION_CONTEXT ( 3 ) GLOBAL_UNCERTAINTY_ASSIGNED_CONTEXT ( ( #5951 ) ) GLOBAL_UNIT_ASSIGNED_CONTEXT ( ( #5359, #4836, #7454 ) ) REPRESENTATION_CONTEXT ( 'NONE', 'WORKASPACE' ) );
#721 = CC_DESIGN_PERSON_AND_ORGANIZATION_ASSIGNMENT ( #8034, #2374, ( #7291 ) ) ;
#722 = LINE ( 'NONE', #3216, #3349 ) ;
#723 = CARTESIAN_POINT ( 'NONE',  ( 0.000000000000000000, 2.359000000000000874, 3.956250000000000266 ) ) ;
#724 = LINE ( 'NONE', #4939, #3752 ) ;
#725 = EDGE_LOOP ( 'NONE', ( #1151, #6212, #424, #2408, #7036, #1194, #6828, #2931, #7258 ) ) ;
#726 = APPLICATION_PROTOCOL_DEFINITION ( 'international standard', 'config_control_design', 1994, #3567 ) ;
#727 = CARTESIAN_POINT ( 'NONE',  ( -8.751021560936518753E-10, 1.000000000000000222, 5.750408897959578548E-10 ) ) ;
#728 = AXIS2_PLACEMENT_3D ( 'NONE', #845, #392, #7206 ) ;
#729 = DIRECTION ( 'NONE',  ( 0.000000000000000000, -0.000000000000000000, 1.000000000000000000 ) ) ;
#730 = EDGE_CURVE ( 'NONE', #4783, #1844, #6554, .T. ) ;
#731 = EDGE_CURVE ( 'NONE', #4455, #1007, #1052, .T. ) ;
#732 = ORIENTED_EDGE ( 'NONE', *, *, #1330, .F. ) ;
#733 = LINE ( 'NONE', #5731, #5536 ) ;
#734 = DIRECTION ( 'NONE',  ( 1.000000000000000000, 0.000000000000000000, 0.000000000000000000 ) ) ;
#735 = EDGE_CURVE ( 'NONE', #2183, #7519, #5964, .T. ) ;
#736 = CARTESIAN_POINT ( 'NONE',  ( -4.462046614173229564, 3.753500037802127043, 8.231249998505111520 ) ) ;
#737 = EDGE_LOOP ( 'NONE', ( #4760, #2818, #4208, #7975 ) ) ;
#738 = FACE_OUTER_BOUND ( 'NONE', #8163, .T. ) ;
#739 = PERSON_AND_ORGANIZATION ( #7862, #8117 ) ;
#740 = EDGE_LOOP ( 'NONE', ( #4028, #158, #2090, #3946 ) ) ;
#741 = DIRECTION ( 'NONE',  ( 1.000000000000000000, 0.000000000000000000, 0.000000000000000000 ) ) ;
#742 = VECTOR ( 'NONE', #5859, 39.37007874015748143 ) ;
#743 = EDGE_CURVE ( 'NONE', #2413, #2164, #1918, .T. ) ;
#744 = VECTOR ( 'NONE', #2267, 39.37007874015748143 ) ;
#745 = CARTESIAN_POINT ( 'NONE',  ( -3.791570908345035740, 1.000000000000000222, 0.7997593681799636256 ) ) ;
#746 = DIRECTION ( 'NONE',  ( -0.000000000000000000, -1.000000000000000000, 0.000000000000000000 ) ) ;
#747 = VECTOR ( 'NONE', #7304, 39.37007874015748854 ) ;
#748 = DIRECTION ( 'NONE',  ( -0.000000000000000000, -1.000000000000000000, -0.000000000000000000 ) ) ;
#749 = FACE_BOUND ( 'NONE', #349, .T. ) ;
#750 = VERTEX_POINT ( 'NONE', #6005 ) ;
#751 = CARTESIAN_POINT ( 'NONE',  ( -2.750000000000000888, 8.719000000000001194, 3.823750000000002647 ) ) ;
#752 = ORIENTED_EDGE ( 'NONE', *, *, #3749, .F. ) ;
#753 = AXIS2_PLACEMENT_3D ( 'NONE', #2039, #4412, #5103 ) ;
#754 = CARTESIAN_POINT ( 'NONE',  ( 3.987953385826771946, 3.776897850680958513, 8.137838423720895165 ) ) ;
#755 = CARTESIAN_POINT ( 'NONE',  ( 1.178157500071308261, 4.528851530234832445, -5.108750000000001457 ) ) ;
#756 = DIRECTION ( 'NONE',  ( -0.000000000000000000, -0.000000000000000000, 1.000000000000000000 ) ) ;
#757 = LINE ( 'NONE', #6249, #7160 ) ;
#758 = EDGE_LOOP ( 'NONE', ( #3244, #6684, #4289, #6147 ) ) ;
#759 = CC_DESIGN_PERSON_AND_ORGANIZATION_ASSIGNMENT ( #5898, #5267, ( #8153 ) ) ;
#760 = FACE_OUTER_BOUND ( 'NONE', #4077, .T. ) ;
#761 = DIRECTION ( 'NONE',  ( 0.000000000000000000, 0.000000000000000000, 1.000000000000000000 ) ) ;
#762 = ORIENTED_EDGE ( 'NONE', *, *, #7780, .T. ) ;
#763 = CALENDAR_DATE ( 2026, 8, 10 ) ;
#764 = DIRECTION ( 'NONE',  ( 0.000000000000000000, 0.000000000000000000, 1.000000000000000000 ) ) ;
#765 = CONTEXT_DEPENDENT_SHAPE_REPRESENTATION ( #951, #3963 ) ;
#766 = DIRECTION ( 'NONE',  ( 0.000000000000000000, 0.000000000000000000, -1.000000000000000000 ) ) ;
#767 = LINE ( 'NONE', #5022, #3826 ) ;
#768 = CC_DESIGN_PERSON_AND_ORGANIZATION_ASSIGNMENT ( #8164, #5724, ( #4741 ) ) ;
#769 = PRODUCT_DEFINITION_SHAPE ( 'NONE', 'NONE',  #3521 ) ;
#770 = ORIENTED_EDGE ( 'NONE', *, *, #2486, .F. ) ;
#771 = DIRECTION ( 'NONE',  ( 0.000000000000000000, 0.000000000000000000, -1.000000000000000000 ) ) ;
#772 = LINE ( 'NONE', #6958, #7989 ) ;
#773 = CARTESIAN_POINT ( 'NONE',  ( -3.987046614173229475, 4.144775419411349304, 8.262149156880317591 ) ) ;
#774 = EDGE_LOOP ( 'NONE', ( #7821, #2662, #6671 ) ) ;
#775 = CARTESIAN_POINT ( 'NONE',  ( -2.750000000000000444, 8.589000000000000412, 5.236250000000000071 ) ) ;
#776 = EDGE_CURVE ( 'NONE', #7088, #2216, #3505, .T. ) ;
#777 = ORIENTED_EDGE ( 'NONE', *, *, #6886, .T. ) ;
#778 = LENGTH_MEASURE_WITH_UNIT ( LENGTH_MEASURE( 0.02539999999999999897 ), #245 );
#779 = CARTESIAN_POINT ( 'NONE',  ( -1.187500000000001110, 4.823637706830838923, 5.420136398917323461 ) ) ;
#780 = PLANE ( 'NONE',  #6507 ) ;
#781 = ADVANCED_FACE ( 'NONE', ( #2884 ), #2847, .F. ) ;
#782 = DATE_AND_TIME ( #1228, #6131 ) ;
#783 = ORIENTED_EDGE ( 'NONE', *, *, #1105, .F. ) ;
#784 = EDGE_CURVE ( 'NONE', #7591, #8139, #5850, .T. ) ;
#785 = DIRECTION ( 'NONE',  ( 0.000000000000000000, 0.000000000000000000, -1.000000000000000000 ) ) ;
#786 = LINE ( 'NONE', #6934, #709 ) ;
#787 = ORIENTED_EDGE ( 'NONE', *, *, #1133, .T. ) ;
#788 = CARTESIAN_POINT ( 'NONE',  ( -3.687499989627467389, 1.365923996832131609E-16, 3.874999999790589289 ) ) ;
#789 = VERTEX_POINT ( 'NONE', #2233 ) ;
#790 = CARTESIAN_POINT ( 'NONE',  ( 3.987953385826772834, 3.862475978536469068, 8.055097764145562778 ) ) ;
#791 = EDGE_CURVE ( 'NONE', #7238, #4179, #7927, .T. ) ;
#792 = CARTESIAN_POINT ( 'NONE',  ( 1.138021836555352051, 4.605302133062858516, -5.108749999999999680 ) ) ;
#793 = ORIENTED_EDGE ( 'NONE', *, *, #5886, .T. ) ;
#794 = DIRECTION ( 'NONE',  ( 0.000000000000000000, 0.000000000000000000, 1.000000000000000000 ) ) ;
#795 = EDGE_LOOP ( 'NONE', ( #4269, #4259, #5089, #128 ) ) ;
#796 = DIRECTION ( 'NONE',  ( -0.000000000000000000, -1.000000000000000000, 0.000000000000000000 ) ) ;
#797 = FACE_OUTER_BOUND ( 'NONE', #1020, .T. ) ;
#798 = ORIENTED_EDGE ( 'NONE', *, *, #7951, .T. ) ;
#799 = SECURITY_CLASSIFICATION_LEVEL ( 'unclassified' ) ;
#800 = CARTESIAN_POINT ( 'NONE',  ( 0.000000000000000000, 1.664000000000000368, 2.841000000000000636 ) ) ;
#801 = PERSON_AND_ORGANIZATION_ROLE ( 'classification_officer' ) ;
#802 = CARTESIAN_POINT ( 'NONE',  ( 2.750000000000000444, 7.964000000000001300, 3.956250000085291152 ) ) ;
#803 = CARTESIAN_POINT ( 'NONE',  ( -2.750000000000000444, 7.964000000000000412, 3.833750000000001545 ) ) ;
#804 = CARTESIAN_POINT ( 'NONE',  ( 0.000000000000000000, 5.339000000000000412, 0.1249999999999997641 ) ) ;
#805 = VERTEX_POINT ( 'NONE', #7201 ) ;
#806 = CARTESIAN_POINT ( 'NONE',  ( -3.987046614173228587, 4.118100097282441752, 8.129275075082505353 ) ) ;
#807 = DIRECTION ( 'NONE',  ( 0.000000000000000000, 0.000000000000000000, 1.000000000000000000 ) ) ;
#808 = CARTESIAN_POINT ( 'NONE',  ( -3.987046614173229475, 4.043411590721250448, 8.404352163763398664 ) ) ;
#809 = ORIENTED_EDGE ( 'NONE', *, *, #688, .F. ) ;
#810 = FACE_OUTER_BOUND ( 'NONE', #795, .T. ) ;
#811 = VERTEX_POINT ( 'NONE', #3585 ) ;
#812 = DIRECTION ( 'NONE',  ( -0.5054526806627168689, -0.8628542794989517706, 0.0002827741471748238282 ) ) ;
#813 = PRODUCT_RELATED_PRODUCT_CATEGORY ( 'detail', '', ( #1182 ) ) ;
#814 = CARTESIAN_POINT ( 'NONE',  ( 2.750000000000000444, 7.521783346456695440, 3.956250000000000266 ) ) ;
#815 = APPLICATION_PROTOCOL_DEFINITION ( 'international standard', 'config_control_design', 1994, #4603 ) ;
#816 = ORIENTED_EDGE ( 'NONE', *, *, #4210, .F. ) ;
#817 = EDGE_CURVE ( 'NONE', #1533, #750, #7991, .T. ) ;
#818 = CARTESIAN_POINT ( 'NONE',  ( 0.000000000000000000, 1.750000000000000444, 2.841000000000000636 ) ) ;
#819 = DIRECTION ( 'NONE',  ( 0.000000000000000000, 1.000000000000000000, 0.000000000000000000 ) ) ;
#820 = CIRCLE ( 'NONE', #5530, 0.3124999879509117728 ) ;
#821 = APPROVAL_DATE_TIME ( #4015, #3007 ) ;
#822 = VERTEX_POINT ( 'NONE', #582 ) ;
#823 = CARTESIAN_POINT ( 'NONE',  ( -0.7499999999999995559, 3.929097005416127608, 7.918750000000000178 ) ) ;
#824 = CC_DESIGN_APPROVAL ( #8089, ( #4347 ) ) ;
#825 = CARTESIAN_POINT ( 'NONE',  ( 0.7122575715994515777, 3.714602561338662401, 8.437773039678205578 ) ) ;
#826 = VECTOR ( 'NONE', #6076, 39.37007874015748143 ) ;
#827 = VECTOR ( 'NONE', #1805, 39.37007874015748143 ) ;
#828 = CARTESIAN_POINT ( 'NONE',  ( 2.537500000000000533, 2.500000000000000444, 0.000000000000000000 ) ) ;
#829 = CARTESIAN_POINT ( 'NONE',  ( 3.987953385826771946, 4.225666661560476989, 7.679916707260901809 ) ) ;
#830 = EDGE_CURVE ( 'NONE', #3439, #3476, #4443, .T. ) ;
#831 = DIRECTION ( 'NONE',  ( 0.7071067811865474617, 0.7071067811865474617, -0.000000000000000000 ) ) ;
#832 = CARTESIAN_POINT ( 'NONE',  ( -4.462046614173229564, 4.146499994074616779, 8.231249998505111520 ) ) ;
#833 = AXIS2_PLACEMENT_3D ( 'NONE', #4893, #1664, #8023 ) ;
#834 = ORIENTED_EDGE ( 'NONE', *, *, #5371, .T. ) ;
#835 = AXIS2_PLACEMENT_3D ( 'NONE', #4211, #503, #1157 ) ;
#836 = ADVANCED_FACE ( 'NONE', ( #1661 ), #6633, .T. ) ;
#837 = AXIS2_PLACEMENT_3D ( 'NONE', #3529, #1073, #949 ) ;
#838 = B_SPLINE_CURVE_WITH_KNOTS ( 'NONE', 3,
 ( #5144, #4414, #6223, #5606 ),
 .UNSPECIFIED., .F., .F.,
 ( 4, 4 ),
 ( 3.040620560812911770E-12, 0.02101476597825354883 ),
 .UNSPECIFIED. ) ;
#839 = AXIS2_PLACEMENT_3D ( 'NONE', #413, #5869, #7269 ) ;
#840 = ADVANCED_FACE ( 'NONE', ( #2198 ), #2152, .T. ) ;
#841 = FACE_OUTER_BOUND ( 'NONE', #3872, .T. ) ;
#842 = DIRECTION ( 'NONE',  ( 0.000000000000000000, 0.000000000000000000, 1.000000000000000000 ) ) ;
#843 = VERTEX_POINT ( 'NONE', #968 ) ;
#844 = PERSON_AND_ORGANIZATION ( #7862, #8117 ) ;
#845 = CARTESIAN_POINT ( 'NONE',  ( 2.875000000000000888, 0.000000000000000000, -2.975000000000000977 ) ) ;
#846 = APPROVAL_ROLE ( '' ) ;
#847 = CARTESIAN_POINT ( 'NONE',  ( 1.500000000000000444, 5.414000000000000590, 0.000000000000000000 ) ) ;
#848 = DIRECTION ( 'NONE',  ( -0.000000000000000000, 0.7071067811865475727, 0.7071067811865475727 ) ) ;
#849 = EDGE_CURVE ( 'NONE', #5226, #7577, #482, .T. ) ;
#850 = AXIS2_PLACEMENT_3D ( 'NONE', #3466, #4604, #924 ) ;
#851 = EDGE_LOOP ( 'NONE', ( #2608, #7946, #1251, #2754, #2509 ) ) ;
#852 = AXIS2_PLACEMENT_3D ( 'NONE', #6468, #1509, #1462 ) ;
#853 = CARTESIAN_POINT ( 'NONE',  ( -3.987046614173228587, 3.806261876195067728, 8.365405826660635924 ) ) ;
#854 = ORIENTED_EDGE ( 'NONE', *, *, #4776, .T. ) ;
#855 = DIRECTION ( 'NONE',  ( 0.000000000000000000, 0.000000000000000000, -1.000000000000000000 ) ) ;
#856 = DIRECTION ( 'NONE',  ( 0.9999998435093852001, 7.428467525934199891E-16, -0.0005594472316430793100 ) ) ;
#857 = LINE ( 'NONE', #246, #1893 ) ;
#858 = AXIS2_PLACEMENT_3D ( 'NONE', #6480, #3914, #812 ) ;
#859 = DIRECTION ( 'NONE',  ( 1.000000000000000000, 0.000000000000000000, -0.000000000000000000 ) ) ;
#860 = APPROVAL_DATE_TIME ( #903, #5459 ) ;
#861 = ORIENTED_EDGE ( 'NONE', *, *, #4247, .T. ) ;
#862 = CC_DESIGN_PERSON_AND_ORGANIZATION_ASSIGNMENT ( #1592, #5853, ( #1882 ) ) ;
#863 = CARTESIAN_POINT ( 'NONE',  ( 1.312500000246545895, 7.352492874015749358, 3.316250000000001474 ) ) ;
#864 = LENGTH_MEASURE_WITH_UNIT ( LENGTH_MEASURE( 0.02539999999999999897 ), #4629 );
#865 = FACE_OUTER_BOUND ( 'NONE', #192, .T. ) ;
#866 = EDGE_LOOP ( 'NONE', ( #2004, #3367, #671, #6711 ) ) ;
#867 = CIRCLE ( 'NONE', #8126, 2.619834094488189269 ) ;
#868 = APPROVAL_ROLE ( '' ) ;
#869 = AXIS2_PLACEMENT_3D ( 'NONE', #7283, #1655, #7234 ) ;
#870 = ORIENTED_EDGE ( 'NONE', *, *, #6187, .F. ) ;
#871 = DIRECTION ( 'NONE',  ( -0.9917930140139561423, 0.000000000000000000, 0.1278538906451907597 ) ) ;
#872 = AXIS2_PLACEMENT_3D ( 'NONE', #4937, #1827, #4319 ) ;
#873 = AXIS2_PLACEMENT_3D ( 'NONE', #5482, #5565, #5028 ) ;
#874 = CARTESIAN_POINT ( 'NONE',  ( -3.791570908345035740, 1.365923996832131609E-16, 0.7997593681799639587 ) ) ;
#875 = CARTESIAN_POINT ( 'NONE',  ( 0.000000000000000000, 2.523992677165354692, 5.972081456692915680 ) ) ;
#876 = PLANE ( 'NONE',  #64 ) ;
#877 = CARTESIAN_POINT ( 'NONE',  ( 3.987953385826772390, 4.143082812052599984, 8.267743937948607069 ) ) ;
#878 = EDGE_CURVE ( 'NONE', #6680, #5163, #6113, .T. ) ;
#879 = EDGE_CURVE ( 'NONE', #41, #5506, #3278, .T. ) ;
#880 = VECTOR ( 'NONE', #2867, 39.37007874015748143 ) ;
#881 = ORIENTED_EDGE ( 'NONE', *, *, #6281, .F. ) ;
#882 = EDGE_CURVE ( 'NONE', #8146, #691, #6317, .T. ) ;
#883 = VECTOR ( 'NONE', #4336, 39.37007874015748143 ) ;
#884 = DIRECTION ( 'NONE',  ( -0.000000000000000000, -0.000000000000000000, 1.000000000000000000 ) ) ;
#885 = CARTESIAN_POINT ( 'NONE',  ( 3.651126734928074491, 1.365923996832131609E-16, -1.298036420927625167 ) ) ;
#886 = ORIENTED_EDGE ( 'NONE', *, *, #5427, .F. ) ;
#887 = EDGE_CURVE ( 'NONE', #2392, #7545, #27, .T. ) ;
#888 = APPROVAL_DATE_TIME ( #3988, #4164 ) ;
#889 = CARTESIAN_POINT ( 'NONE',  ( 0.7499999999999993339, 3.950000000000000178, 8.831250000000000711 ) ) ;
#890 = APPROVAL_DATE_TIME ( #6518, #7812 ) ;
#891 = DIRECTION ( 'NONE',  ( 1.000000000000000000, -0.000000000000000000, 0.000000000000000000 ) ) ;
#892 = DIRECTION ( 'NONE',  ( -0.000000000000000000, -1.000000000000000000, 0.000000000000000000 ) ) ;
#893 = LOCAL_TIME ( 0, 37, 23.00000000000000000, #4585 ) ;
#894 = ORIENTED_EDGE ( 'NONE', *, *, #2407, .F. ) ;
#895 = FACE_OUTER_BOUND ( 'NONE', #1335, .T. ) ;
#896 = DIRECTION ( 'NONE',  ( -0.000000000000000000, -0.000000000000000000, 1.000000000000000000 ) ) ;
#897 = DIRECTION ( 'NONE',  ( 0.000000000000000000, 0.000000000000000000, 1.000000000000000000 ) ) ;
#898 = CARTESIAN_POINT ( 'NONE',  ( 1.462953684461641091, 1.365923996832131609E-16, 3.588229578933126440 ) ) ;
#899 = ADVANCED_FACE ( 'NONE', ( #3362, #3282 ), #2975, .T. ) ;
#900 = ORIENTED_EDGE ( 'NONE', *, *, #5752, .F. ) ;
#901 = CARTESIAN_POINT ( 'NONE',  ( -8.751021560936518753E-10, 1.000000000000000222, 5.750408897959578548E-10 ) ) ;
#902 = DIRECTION ( 'NONE',  ( -7.142086257945775577E-16, -1.000000000000000000, 0.000000000000000000 ) ) ;
#903 = DATE_AND_TIME ( #656, #5605 ) ;
#904 = ORIENTED_EDGE ( 'NONE', *, *, #3972, .F. ) ;
#905 = APPLICATION_CONTEXT ( 'configuration controlled 3d designs of mechanical parts and assemblies' ) ;
#906 = CARTESIAN_POINT ( 'NONE',  ( 0.000000000000000000, 1.664000000000000368, 2.693920355039552791E-42 ) ) ;
#907 = DIRECTION ( 'NONE',  ( 0.000000000000000000, 1.000000000000000000, 0.000000000000000000 ) ) ;
#908 =( CONVERSION_BASED_UNIT ( 'INCH', #7100 ) LENGTH_UNIT ( ) NAMED_UNIT ( #4284 ) );
#909 = CARTESIAN_POINT ( 'NONE',  ( -1.074999999999999289, 3.950000000000000178, 3.440250000000000696 ) ) ;
#910 = ORIENTED_EDGE ( 'NONE', *, *, #1941, .F. ) ;
#911 = PERSON_AND_ORGANIZATION ( #7862, #8117 ) ;
#912 = EDGE_LOOP ( 'NONE', ( #8131, #2717 ) ) ;
#913 = FACE_OUTER_BOUND ( 'NONE', #7401, .T. ) ;
#914 = CARTESIAN_POINT ( 'NONE',  ( -2.740000000000001545, 8.729000000000002757, 4.313750000000002416 ) ) ;
#915 = CARTESIAN_POINT ( 'NONE',  ( 3.987953385826771946, 4.146499994074615891, 8.231249998505111520 ) ) ;
#916 = CARTESIAN_POINT ( 'NONE',  ( -3.224046040006844027, 0.9999999999998147038, -2.215849741854215793 ) ) ;
#917 = ORIENTED_EDGE ( 'NONE', *, *, #5026, .F. ) ;
#918 = CC_DESIGN_PERSON_AND_ORGANIZATION_ASSIGNMENT ( #1911, #5634, ( #7802 ) ) ;
#919 = CARTESIAN_POINT ( 'NONE',  ( 3.987953385826772834, 4.112654374748815123, 8.341552593656999193 ) ) ;
#920 = ORIENTED_EDGE ( 'NONE', *, *, #7725, .T. ) ;
#921 = EDGE_CURVE ( 'NONE', #7981, #7410, #5112, .T. ) ;
#922 = DIRECTION ( 'NONE',  ( -0.000000000000000000, 1.000000000000000000, -0.000000000000000000 ) ) ;
#923 = LINE ( 'NONE', #3422, #5293 ) ;
#924 = DIRECTION ( 'NONE',  ( -0.000000000000000000, 0.000000000000000000, -1.000000000000000000 ) ) ;
#925 = APPLICATION_PROTOCOL_DEFINITION ( 'international standard', 'config_control_design', 1994, #905 ) ;
#926 = EDGE_CURVE ( 'NONE', #2164, #605, #7448, .T. ) ;
#927 = LINE ( 'NONE', #5920, #3990 ) ;
#928 = APPROVAL_STATUS ( 'not_yet_approved' ) ;
#929 = CARTESIAN_POINT ( 'NONE',  ( 0.7122963468828457101, 3.714722057770372565, 8.024595996655376595 ) ) ;
#930 = DIRECTION ( 'NONE',  ( 0.000000000000000000, -1.000000000000000000, 0.000000000000000000 ) ) ;
#931 = DIRECTION ( 'NONE',  ( -1.000000000000000000, -0.000000000000000000, -0.000000000000000000 ) ) ;
#932 = LOCAL_TIME ( 0, 37, 23.00000000000000000, #5679 ) ;
#933 = ORIENTED_EDGE ( 'NONE', *, *, #6659, .T. ) ;
#934 = FACE_OUTER_BOUND ( 'NONE', #5620, .T. ) ;
#935 = CARTESIAN_POINT ( 'NONE',  ( -3.987046614173229919, 4.133273763909712351, 8.302127249793111119 ) ) ;
#936 = EDGE_LOOP ( 'NONE', ( #5279, #1727, #4391, #1423 ) ) ;
#937 = CARTESIAN_POINT ( 'NONE',  ( -2.150000000000000799, 2.875000000000000888, 3.440250000000000696 ) ) ;
#938 = VERTEX_POINT ( 'NONE', #7905 ) ;
#939 = DIRECTION ( 'NONE',  ( 0.000000000000000000, 0.000000000000000000, -1.000000000000000000 ) ) ;
#940 = PERSON_AND_ORGANIZATION ( #7862, #8117 ) ;
#941 = VERTEX_POINT ( 'NONE', #6099 ) ;
#942 = EDGE_CURVE ( 'NONE', #1477, #5222, #5980, .T. ) ;
#943 = EDGE_CURVE ( 'NONE', #3948, #8045, #8127, .T. ) ;
#944 = CARTESIAN_POINT ( 'NONE',  ( -1.138021853580373666, 3.294697891665690825, -5.108749999999999680 ) ) ;
#945 = LINE ( 'NONE', #7829, #4536 ) ;
#946 = DIRECTION ( 'NONE',  ( -0.000000000000000000, 0.000000000000000000, 1.000000000000000000 ) ) ;
#947 = B_SPLINE_CURVE_WITH_KNOTS ( 'NONE', 3,
 ( #5498, #8149, #3779, #4348, #2484, #7548, #1129, #6200, #1896, #3164, #2447, #6856, #508, #5539, #8061, #2397, #1854, #7426, #1785, #8107, #4469, #3290, #5169, #1325, #7628, #4431, #4512, #3928, #1981, #7067, #1942, #7028, #6325, #6368, #4598, #6939, #6982, #7108, #4557, #790, #5788, #167, #2019, #217, #1371, #3813, #7752, #1452, #1495, #6453, #3854, #754, #1414, #2597, #711, #3247, #2558, #6410, #2719, #5126, #5090, #3206, #5876, #5048, #5207, #5750 ),
 .UNSPECIFIED., .F., .F.,
 ( 4, 1, 1, 1, 1, 2, 2, 1, 2, 2, 2, 1, 2, 2, 1, 1, 1, 2, 2, 2, 1, 1, 1, 1, 2, 2, 1, 2, 2, 2, 1, 2, 2, 1, 1, 2, 2, 1, 1, 1, 2, 2, 4 ),
 ( 0.000000000000000000, 0.06249999999998323563, 0.09374999999997758737, 0.1093749999999724942, 0.1171874999999721056, 0.1210937499999718975, 0.1249999999999717171, 0.1562499999999758249, 0.1718749999999749922, 0.1874999999999741596, 0.2499999999999581446, 0.2812499999999501510, 0.2968749999999454880, 0.3124999999999408806, 0.3437499999999316658, 0.3593749999999270028, 0.3671874999999247269, 0.3710937499999257816, 0.3749999999999268363, 0.4999999999999173994, 0.5624999999999127365, 0.5937499999999102940, 0.6093749999999091838, 0.6171874999999095168, 0.6210937499999082956, 0.6249999999999071854, 0.6562499999999119593, 0.6718749999999144018, 0.6874999999999167333, 0.7499999999999256151, 0.7812499999999300559, 0.7968749999999323874, 0.8124999999999346079, 0.8437499999999376055, 0.8593749999999362732, 0.8671874999999384936, 0.8749999999999407141, 0.9062499999999484857, 0.9218749999999550360, 0.9296874999999605871, 0.9335937499999659162, 0.9374999999999713562, 1.000000000000000000 ),
 .UNSPECIFIED. ) ;
#948 =( NAMED_UNIT ( * ) SI_UNIT ( $, .STERADIAN. ) SOLID_ANGLE_UNIT ( ) );
#949 = DIRECTION ( 'NONE',  ( 0.000000000000000000, 0.000000000000000000, 1.000000000000000000 ) ) ;
#950 = CALENDAR_DATE ( 2026, 8, 10 ) ;
#951 =( REPRESENTATION_RELATIONSHIP ('NONE','NONE', #3570, #6969 ) REPRESENTATION_RELATIONSHIP_WITH_TRANSFORMATION ( #2733 )SHAPE_REPRESENTATION_RELATIONSHIP( ) );
#952 = ORIENTED_EDGE ( 'NONE', *, *, #6340, .T. ) ;
#953 = CARTESIAN_POINT ( 'NONE',  ( -3.796513189164428148, 1.000000000000000666, -2.946478859991636057 ) ) ;
#954 = CARTESIAN_POINT ( 'NONE',  ( 0.7491228847736894902, 3.908369212101149071, 8.541661844804181669 ) ) ;
#955 = UNCERTAINTY_MEASURE_WITH_UNIT (LENGTH_MEASURE( 1.000000000000000082E-05 ), #2427, 'distance_accuracy_value', 'NONE');
#956 = ADVANCED_FACE ( 'NONE', ( #2283 ), #2211, .T. ) ;
#957 = DIRECTION ( 'NONE',  ( 1.000000000000000000, 0.000000000000000000, -0.000000000000000000 ) ) ;
#958 = DIRECTION ( 'NONE',  ( -0.7071067811865554553, 1.583668658704876446E-14, -0.7071067811865395791 ) ) ;
#959 = ADVANCED_FACE ( 'N', ( #2980 ), #4782, .T. ) ;
#960 = CC_DESIGN_APPROVAL ( #6229, ( #3944 ) ) ;
#961 = ORIENTED_EDGE ( 'NONE', *, *, #5735, .F. ) ;
#962 = CARTESIAN_POINT ( 'NONE',  ( 3.987953385826772390, 4.051924899703798211, 8.399281692864075666 ) ) ;
#963 = VERTEX_POINT ( 'NONE', #7388 ) ;
#964 = AXIS2_PLACEMENT_3D ( 'NONE', #138, #4485, #3348 ) ;
#965 = LOCAL_TIME ( 0, 37, 23.00000000000000000, #1252 ) ;
#966 = CC_DESIGN_DATE_AND_TIME_ASSIGNMENT ( #6927, #2548, ( #3856 ) ) ;
#967 = CARTESIAN_POINT ( 'NONE',  ( -3.987046614173228587, 4.130163526686910558, 8.152788242568700383 ) ) ;
#968 = CARTESIAN_POINT ( 'NONE',  ( 1.500000000000000444, 5.414000000000000590, 2.750000000234376074 ) ) ;
#969 = CARTESIAN_POINT ( 'NONE',  ( -8.751021560936518753E-10, 1.000000000000000222, 5.750408897959578548E-10 ) ) ;
#970 = VECTOR ( 'NONE', #2759, 39.37007874015748143 ) ;
#971 = DIRECTION ( 'NONE',  ( 0.7071067811865395791, -5.050217624812654886E-16, 0.7071067811865554553 ) ) ;
#972 = DIRECTION ( 'NONE',  ( -0.000000000000000000, 1.000000000000000000, -0.000000000000000000 ) ) ;
#973 = APPROVAL_DATE_TIME ( #3298, #1862 ) ;
#974 = VECTOR ( 'NONE', #5005, 39.37007874015748143 ) ;
#975 = CYLINDRICAL_SURFACE ( 'NONE', #5703, 1.074999999999999289 ) ;
#976 = APPROVAL_ROLE ( '' ) ;
#977 = CARTESIAN_POINT ( 'NONE',  ( 0.6818077110526902240, 4.262471192484426297, 8.252326836086270490 ) ) ;
#978 = DIRECTION ( 'NONE',  ( 0.000000000000000000, -1.000000000000000000, 0.000000000000000000 ) ) ;
#979 = CARTESIAN_POINT ( 'NONE',  ( 2.750000000000002665, 8.589000000000000412, 3.161250000000001670 ) ) ;
#980 = AXIS2_PLACEMENT_3D ( 'NONE', #7572, #3273, #2582 ) ;
#981 = EDGE_LOOP ( 'NONE', ( #1160, #4241, #22, #3595, #17 ) ) ;
#982 = AXIS2_PLACEMENT_3D ( 'NONE', #6039, #6734, #422 ) ;
#983 = DIRECTION ( 'NONE',  ( 0.000000000000000000, 0.000000000000000000, -1.000000000000000000 ) ) ;
#984 = ORIENTED_EDGE ( 'NONE', *, *, #7546, .F. ) ;
#985 = CARTESIAN_POINT ( 'NONE',  ( 2.537499998660271761, 3.550000000000001155, 2.790532913385826763 ) ) ;
#986 = DIRECTION ( 'NONE',  ( 0.000000000000000000, 0.000000000000000000, 1.000000000000000000 ) ) ;
#987 = VERTEX_POINT ( 'NONE', #4240 ) ;
#988 = PERSON_AND_ORGANIZATION ( #7862, #8117 ) ;
#989 = CARTESIAN_POINT ( 'NONE',  ( 3.651126735575231042, 1.000000000000000222, -1.298036422080803165 ) ) ;
#990 = DATE_TIME_ROLE ( 'classification_date' ) ;
#991 = EDGE_LOOP ( 'NONE', ( #6821, #1517, #4310 ) ) ;
#992 = CIRCLE ( 'NONE', #1895, 1.624999999999999778 ) ;
#993 = ADVANCED_FACE ( 'NONE', ( #4072 ), #4698, .F. ) ;
#994 = CARTESIAN_POINT ( 'NONE',  ( -1.303938013533521678, 4.122802601861688565, -5.108750000000004121 ) ) ;
#995 = DIRECTION ( 'NONE',  ( -0.000000000000000000, -0.7071067811865475727, -0.7071067811865475727 ) ) ;
#996 = CARTESIAN_POINT ( 'NONE',  ( -1.312500000000000444, 8.589000000000000412, 2.411250000000000782 ) ) ;
#997 = APPLICATION_PROTOCOL_DEFINITION ( 'international standard', 'config_control_design', 1994, #4294 ) ;
#998 = ORIENTED_EDGE ( 'NONE', *, *, #2689, .T. ) ;
#999 = CARTESIAN_POINT ( 'NONE',  ( -3.362500000000001155, 1.750000000000000444, 4.117874862132976456E-16 ) ) ;
#1000 = AXIS2_PLACEMENT_3D ( 'NONE', #4934, #4894, #669 ) ;
#1001 =( GEOMETRIC_REPRESENTATION_CONTEXT ( 3 ) GLOBAL_UNCERTAINTY_ASSIGNED_CONTEXT ( ( #6625 ) ) GLOBAL_UNIT_ASSIGNED_CONTEXT ( ( #4700, #3879, #6571 ) ) REPRESENTATION_CONTEXT ( 'NONE', 'WORKASPACE' ) );
#1002 = LINE ( 'NONE', #2878, #3964 ) ;
#1003 = CARTESIAN_POINT ( 'NONE',  ( -1.500000000000000444, 5.414000000000000590, 0.000000000000000000 ) ) ;
#1004 = FACE_OUTER_BOUND ( 'NONE', #7933, .T. ) ;
#1005 = EDGE_CURVE ( 'NONE', #1089, #4859, #358, .T. ) ;
#1006 = DIRECTION ( 'NONE',  ( -0.000000000000000000, 1.000000000000000000, -0.000000000000000000 ) ) ;
#1007 = VERTEX_POINT ( 'NONE', #6792 ) ;
#1008 = CARTESIAN_POINT ( 'NONE',  ( -3.987046614173228587, 4.079363137579387733, 8.082722253684375247 ) ) ;
#1009 = CARTESIAN_POINT ( 'NONE',  ( 2.750000000000000444, 8.719000000000002970, 3.823750000000002647 ) ) ;
#1010 = CARTESIAN_POINT ( 'NONE',  ( -2.750000000000000888, 7.964000000000000412, 3.333750000000001990 ) ) ;
#1011 = DIRECTION ( 'NONE',  ( -0.000000000000000000, 1.000000000000000000, -0.000000000000000000 ) ) ;
#1012 = FACE_OUTER_BOUND ( 'NONE', #1498, .T. ) ;
#1013 = ORIENTED_EDGE ( 'NONE', *, *, #3353, .F. ) ;
#1014 = AXIS2_PLACEMENT_3D ( 'NONE', #1065, #3557, #4200 ) ;
#1015 = PERSON_AND_ORGANIZATION ( #7862, #8117 ) ;
#1016 = CARTESIAN_POINT ( 'NONE',  ( -3.796513189164426816, 1.365923996832131609E-16, -2.946478859991635169 ) ) ;
#1017 = CC_DESIGN_PERSON_AND_ORGANIZATION_ASSIGNMENT ( #3486, #7218, ( #1774 ) ) ;
#1018 = CARTESIAN_POINT ( 'NONE',  ( 1.312500000000000222, 7.339000000000000412, 3.239595687480216313 ) ) ;
#1019 = VECTOR ( 'NONE', #3073, 39.37007874015748143 ) ;
#1020 = EDGE_LOOP ( 'NONE', ( #1948, #5905, #4612, #7659 ) ) ;
#1021 = LINE ( 'NONE', #437, #3102 ) ;
#1022 = CARTESIAN_POINT ( 'NONE',  ( -1.625000000000000222, 5.339000000000000412, 0.1250000000000000278 ) ) ;
#1023 = CARTESIAN_POINT ( 'NONE',  ( 0.000000000000000000, 5.238734212598425088, 3.956250000000001155 ) ) ;
#1024 = ORIENTED_EDGE ( 'NONE', *, *, #1386, .T. ) ;
#1025 = PERSON_AND_ORGANIZATION ( #7862, #8117 ) ;
#1026 = DIRECTION ( 'NONE',  ( 1.000000000000000000, 0.000000000000000000, -0.000000000000000000 ) ) ;
#1027 = CARTESIAN_POINT ( 'NONE',  ( 2.537499998660271761, 3.550000000000001155, -0.3883559095726498156 ) ) ;
#1028 = CONTEXT_DEPENDENT_SHAPE_REPRESENTATION ( #6399, #524 ) ;
#1029 = ORIENTED_EDGE ( 'NONE', *, *, #3972, .T. ) ;
#1030 = PRODUCT_DEFINITION ( 'UNKNOWN', '', #2798, #3569 ) ;
#1031 = CC_DESIGN_APPROVAL ( #5459, ( #8153 ) ) ;
#1032 = CARTESIAN_POINT ( 'NONE',  ( -1.282759086114038771, 4.228660313282746053, -5.108750000000003233 ) ) ;
#1033 = DIRECTION ( 'NONE',  ( 1.000000000000000000, 0.000000000000000000, 0.000000000000000000 ) ) ;
#1034 = CARTESIAN_POINT ( 'NONE',  ( -2.750000000000000444, 7.521783346456695440, 3.691250000000001030 ) ) ;
#1035 = EDGE_CURVE ( 'NONE', #843, #4996, #7483, .T. ) ;
#1036 =( NAMED_UNIT ( * ) SI_UNIT ( $, .STERADIAN. ) SOLID_ANGLE_UNIT ( ) );
#1037 = PLANE ( 'NONE',  #576 ) ;
#1038 = APPROVAL_STATUS ( 'not_yet_approved' ) ;
#1039 = EDGE_LOOP ( 'NONE', ( #933, #4900, #258, #5263, #375, #6338, #2581, #3852 ) ) ;
#1040 = ADVANCED_FACE ( 'NONE', ( #4904 ), #1334, .T. ) ;
#1041 = DIRECTION ( 'NONE',  ( 1.000000000000000000, 0.000000000000000000, -0.000000000000000000 ) ) ;
#1042 = LOCAL_TIME ( 0, 37, 23.00000000000000000, #7135 ) ;
#1043 = DIRECTION ( 'NONE',  ( 0.000000000000000000, 0.000000000000000000, -1.000000000000000000 ) ) ;
#1044 = LINE ( 'NONE', #6814, #4354 ) ;
#1045 = DIRECTION ( 'NONE',  ( 0.000000000000000000, -0.000000000000000000, 1.000000000000000000 ) ) ;
#1046 = CARTESIAN_POINT ( 'NONE',  ( 2.745000000000000995, 7.974000000000001087, 3.818750000000002753 ) ) ;
#1047 = CARTESIAN_POINT ( 'NONE',  ( -0.6892550738286248313, 3.654300326837817803, 8.332856313163134132 ) ) ;
#1048 = ORIENTED_EDGE ( 'NONE', *, *, #4471, .T. ) ;
#1049 = EDGE_CURVE ( 'NONE', #1962, #3600, #3677, .T. ) ;
#1050 = DIRECTION ( 'NONE',  ( 0.000000000000000000, 0.000000000000000000, -1.000000000000000000 ) ) ;
#1051 = CARTESIAN_POINT ( 'NONE',  ( -3.987046614173229475, 4.020876854703656633, 8.047976087269148593 ) ) ;
#1052 = LINE ( 'NONE', #1009, #5446 ) ;
#1053 = CARTESIAN_POINT ( 'NONE',  ( 3.296097360985625002, 1.750000000000000444, 0.5624999982029994516 ) ) ;
#1054 = ORIENTED_EDGE ( 'NONE', *, *, #6520, .T. ) ;
#1055 = APPROVAL_STATUS ( 'not_yet_approved' ) ;
#1056 = FACE_OUTER_BOUND ( 'NONE', #4658, .T. ) ;
#1057 = CARTESIAN_POINT ( 'NONE',  ( 1.312500000000000222, 7.339000000000001300, 3.161250000000001670 ) ) ;
#1058 = SECURITY_CLASSIFICATION ( '', '', #7727 ) ;
#1059 = VERTEX_POINT ( 'NONE', #5597 ) ;
#1060 = EDGE_LOOP ( 'NONE', ( #3167, #7736 ) ) ;
#1061 = FACE_OUTER_BOUND ( 'NONE', #2906, .T. ) ;
#1062 = ORIENTED_EDGE ( 'NONE', *, *, #6498, .F. ) ;
#1063 = CALENDAR_DATE ( 2026, 8, 10 ) ;
#1064 = DIRECTION ( 'NONE',  ( 0.000000000000000000, -0.7071067811865475727, 0.7071067811865475727 ) ) ;
#1065 = CARTESIAN_POINT ( 'NONE',  ( -8.751021560936518753E-10, 1.000000000000000222, 5.750408897959578548E-10 ) ) ;
#1066 = PERSON_AND_ORGANIZATION ( #7231, #2753 ) ;
#1067 = ORIENTED_EDGE ( 'NONE', *, *, #6553, .F. ) ;
#1068 = CYLINDRICAL_SURFACE ( 'NONE', #348, 0.3124999879509117728 ) ;
#1069 = PLANE ( 'NONE',  #4362 ) ;
#1070 = CC_DESIGN_DATE_AND_TIME_ASSIGNMENT ( #5873, #2791, ( #7674 ) ) ;
#1071 = CARTESIAN_POINT ( 'NONE',  ( -0.7370170160409599269, 4.089247961470974246, 8.511197325751677312 ) ) ;
#1072 =( LENGTH_UNIT ( ) NAMED_UNIT ( * ) SI_UNIT ( $, .METRE. ) );
#1073 = DIRECTION ( 'NONE',  ( -1.000000000000000000, 0.000000000000000000, 0.000000000000000000 ) ) ;
#1074 = APPROVAL_ROLE ( '' ) ;
#1075 = ORIENTED_EDGE ( 'NONE', *, *, #4838, .F. ) ;
#1076 = CARTESIAN_POINT ( 'NONE',  ( -4.462046614173229564, 4.146499994075096396, 7.838250042231664771 ) ) ;
#1077 = EDGE_CURVE ( 'NONE', #674, #3226, #4552, .T. ) ;
#1078 = DIRECTION ( 'NONE',  ( 1.000000000000000000, 0.000000000000000000, 0.000000000000000000 ) ) ;
#1079 = CARTESIAN_POINT ( 'NONE',  ( 1.500000000000000444, 5.969165905511811587, 0.5414159055118110686 ) ) ;
#1080 = VERTEX_POINT ( 'NONE', #1908 ) ;
#1081 = CARTESIAN_POINT ( 'NONE',  ( -1.187500000000000222, 5.969165905511811587, 4.238473622047244760 ) ) ;
#1082 = EDGE_CURVE ( 'NONE', #5017, #5232, #7856, .T. ) ;
#1083 = ORIENTED_EDGE ( 'NONE', *, *, #2557, .T. ) ;
#1084 = ADVANCED_FACE ( 'NONE', ( #5554 ), #644, .F. ) ;
#1085 = EDGE_CURVE ( 'NONE', #2688, #5456, #679, .T. ) ;
#1086 = FACE_OUTER_BOUND ( 'NONE', #2054, .T. ) ;
#1087 = CARTESIAN_POINT ( 'NONE',  ( 1.625000000000000222, 5.639000000000001123, -2.908930215307243383 ) ) ;
#1088 = DIRECTION ( 'NONE',  ( 0.08785522361217637521, 0.000000000000000000, -0.9961332539796342589 ) ) ;
#1089 = VERTEX_POINT ( 'NONE', #4 ) ;
#1090 = COORDINATED_UNIVERSAL_TIME_OFFSET ( 0, 0, .AHEAD. ) ;
#1091 = PLANE ( 'NONE',  #470 ) ;
#1092 = ADVANCED_FACE ( 'NONE', ( #8121 ), #53, .F. ) ;
#1093 = VECTOR ( 'NONE', #2380, 39.37007874015748854 ) ;
#1094 = CARTESIAN_POINT ( 'NONE',  ( -1.172489671586610660, 1.365923996832131609E-16, -3.693357951819909779 ) ) ;
#1095 = CC_DESIGN_APPROVAL ( #666, ( #4741 ) ) ;
#1096 = ORIENTED_EDGE ( 'NONE', *, *, #3735, .F. ) ;
#1097 = CIRCLE ( 'NONE', #5667, 1.124999999999999556 ) ;
#1098 = VECTOR ( 'NONE', #4453, 39.37007874015748143 ) ;
#1099 = CARTESIAN_POINT ( 'NONE',  ( -2.740000000000000213, 8.719000000000001194, 3.323750000000001759 ) ) ;
#1100 = ORIENTED_EDGE ( 'NONE', *, *, #4193, .T. ) ;
#1101 = DIRECTION ( 'NONE',  ( 1.000000000000000000, 0.000000000000000000, 0.000000000000000000 ) ) ;
#1102 = CARTESIAN_POINT ( 'NONE',  ( 4.383786719160104539, 3.516000035344543750, 8.231249998505111520 ) ) ;
#1103 = B_SPLINE_CURVE_WITH_KNOTS ( 'NONE', 3,
 ( #5274, #4045, #6687, #6065, #451, #330 ),
 .UNSPECIFIED., .F., .F.,
 ( 4, 2, 4 ),
 ( 0.000000000000000000, 0.5000000000000000000, 1.000000000000000000 ),
 .UNSPECIFIED. ) ;
#1104 = CALENDAR_DATE ( 2026, 8, 10 ) ;
#1105 = EDGE_CURVE ( 'NONE', #6766, #3004, #1148, .T. ) ;
#1106 = ORIENTED_EDGE ( 'NONE', *, *, #3888, .T. ) ;
#1107 = VECTOR ( 'NONE', #6433, 39.37007874015748143 ) ;
#1108 = APPLICATION_CONTEXT ( 'configuration controlled 3d designs of mechanical parts and assemblies' ) ;
#1109 = LINE ( 'NONE', #7357, #827 ) ;
#1110 = AXIS2_PLACEMENT_3D ( 'NONE', #6443, #819, #157 ) ;
#1111 = CARTESIAN_POINT ( 'NONE',  ( -0.7210672075785411472, 4.156465442921959408, 7.996449899345011048 ) ) ;
#1112 =( BOUNDED_CURVE ( )  B_SPLINE_CURVE ( 3, ( #5649, #7059, #1443, #74 ),
 .UNSPECIFIED., .F., .F. ) 
 B_SPLINE_CURVE_WITH_KNOTS ( ( 4, 4 ),
 ( 0.000000000000000000, 1.000000000000000000 ),
 .UNSPECIFIED. ) 
 CURVE ( )  GEOMETRIC_REPRESENTATION_ITEM ( )  RATIONAL_B_SPLINE_CURVE ( ( 1.000000000000000000, 0.3333333333333334259, 0.3333333333333334259, 1.000000000000000000 ) ) 
 REPRESENTATION_ITEM ( '' )  );
#1113 = VECTOR ( 'NONE', #2570, 39.37007874015748143 ) ;
#1114 = DIRECTION ( 'NONE',  ( 0.000000000000000000, -0.000000000000000000, 1.000000000000000000 ) ) ;
#1115 = CIRCLE ( 'NONE', #982, 0.7499999999999993339 ) ;
#1116 = DATE_TIME_ROLE ( 'classification_date' ) ;
#1117 = VERTEX_POINT ( 'NONE', #2461 ) ;
#1118 = CARTESIAN_POINT ( 'NONE',  ( 0.000000000000000000, 7.973999999999999311, 4.323750000000001315 ) ) ;
#1119 = CC_DESIGN_DATE_AND_TIME_ASSIGNMENT ( #7764, #7684, ( #600 ) ) ;
#1120 =( GEOMETRIC_REPRESENTATION_CONTEXT ( 3 ) GLOBAL_UNCERTAINTY_ASSIGNED_CONTEXT ( ( #4051 ) ) GLOBAL_UNIT_ASSIGNED_CONTEXT ( ( #5826, #3965, #1036 ) ) REPRESENTATION_CONTEXT ( 'NONE', 'WORKASPACE' ) );
#1121 = ORIENTED_EDGE ( 'NONE', *, *, #8052, .T. ) ;
#1122 = DIRECTION ( 'NONE',  ( 0.000000000000000000, 1.000000000000000000, 0.000000000000000000 ) ) ;
#1123 = DIRECTION ( 'NONE',  ( 1.000000000000000000, 0.000000000000000000, 0.000000000000000000 ) ) ;
#1124 = ORIENTED_EDGE ( 'NONE', *, *, #4724, .F. ) ;
#1125 = CARTESIAN_POINT ( 'NONE',  ( -1.201750196850394081, 2.500000000000000444, -2.750000000000000444 ) ) ;
#1126 = ORIENTED_EDGE ( 'NONE', *, *, #5708, .F. ) ;
#1127 = B_SPLINE_CURVE_WITH_KNOTS ( 'NONE', 3,
 ( #1436, #280, #773, #6431, #7733, #5146, #3876, #935, #4035, #7171, #2046, #6567, #7770, #4613, #5225, #2774, #2087, #7051, #7648, #5262, #1471, #7818, #808, #6390, #3396, #4577, #105, #3271, #5893, #5189, #196, #6477, #2619, #4494, #7087, #7007, #1516, #4540, #2167, #4655, #1394, #1555, #5771, #3945, #2738, #853, #3354, #5812, #7127, #5860, #4000, #2705, #242, #6526, #7694, #145, #3910, #3308, #2122, #2661, #5540, #5461, #4852, #3665, #4349, #4891 ),
 .UNSPECIFIED., .F., .F.,
 ( 4, 1, 1, 1, 1, 2, 2, 1, 2, 2, 2, 1, 2, 2, 1, 1, 1, 2, 2, 2, 1, 1, 1, 1, 2, 2, 1, 2, 2, 2, 1, 2, 2, 1, 1, 2, 2, 1, 1, 1, 2, 2, 4 ),
 ( 0.000000000000000000, 0.06250000000002353673, 0.09375000000003830269, 0.1093750000000430211, 0.1171875000000484335, 0.1210937500000485584, 0.1250000000000486833, 0.1562500000000372757, 0.1718750000000286715, 0.1875000000000200673, 0.2499999999999983347, 0.2812499999999865663, 0.2968749999999816813, 0.3124999999999767963, 0.3437499999999648614, 0.3593749999999588662, 0.3671874999999570344, 0.3710937499999559241, 0.3749999999999548694, 0.4999999999999330536, 0.5624999999999207301, 0.5937499999999150679, 0.6093749999999122924, 0.6171874999999112932, 0.6210937499999130695, 0.6249999999999147349, 0.6562499999999166223, 0.6718749999999176215, 0.6874999999999186207, 0.7499999999999197309, 0.7812499999999220623, 0.7968749999999220623, 0.8124999999999220623, 0.8437499999999235056, 0.8593749999999270583, 0.8671874999999292788, 0.8749999999999316103, 0.9062499999999429345, 0.9218749999999511502, 0.9296874999999525935, 0.9335937499999537037, 0.9374999999999547029, 1.000000000000000000 ),
 .UNSPECIFIED. ) ;
#1128 = AXIS2_PLACEMENT_3D ( 'NONE', #1669, #6786, #7300 ) ;
#1129 = CARTESIAN_POINT ( 'NONE',  ( 3.987953385826773278, 4.133830657811393472, 8.161828647664988168 ) ) ;
#1130 = DIRECTION ( 'NONE',  ( -0.7071067811865474617, 0.000000000000000000, -0.7071067811865474617 ) ) ;
#1131 = CARTESIAN_POINT ( 'NONE',  ( 2.750000000000000888, 8.719000000000001194, 3.333750000000001990 ) ) ;
#1132 = CARTESIAN_POINT ( 'NONE',  ( 1.187499999999999778, 4.331466137858002163, 6.700178998068949454 ) ) ;
#1133 = EDGE_CURVE ( 'NONE', #3502, #5894, #724, .T. ) ;
#1134 = EDGE_LOOP ( 'NONE', ( #6358, #6595, #7126, #4769 ) ) ;
#1135 = APPROVAL_ROLE ( '' ) ;
#1136 = CARTESIAN_POINT ( 'NONE',  ( 0.000000000000000000, 0.000000000000000000, 0.1249999999999997641 ) ) ;
#1137 = ADVANCED_FACE ( 'NONE', ( #363 ), #5351, .T. ) ;
#1138 = ORIENTED_EDGE ( 'NONE', *, *, #1704, .F. ) ;
#1139 = AXIS2_PLACEMENT_3D ( 'NONE', #3516, #278, #2773 ) ;
#1140 = LINE ( 'NONE', #1863, #619 ) ;
#1141 = DIRECTION ( 'NONE',  ( 0.000000000000000000, 0.000000000000000000, 1.000000000000000000 ) ) ;
#1142 = ORIENTED_EDGE ( 'NONE', *, *, #7781, .T. ) ;
#1143 = APPLICATION_PROTOCOL_DEFINITION ( 'international standard', 'config_control_design', 1994, #6968 ) ;
#1144 = DIRECTION ( 'NONE',  ( 0.000000000000000000, -0.000000000000000000, 1.000000000000000000 ) ) ;
#1145 = CONTEXT_DEPENDENT_SHAPE_REPRESENTATION ( #94, #4315 ) ;
#1146 = LINE ( 'NONE', #4789, #3871 ) ;
#1147 = CARTESIAN_POINT ( 'NONE',  ( 2.537499998660271761, 3.550000000000001155, -0.3883559095726498156 ) ) ;
#1148 = CIRCLE ( 'NONE', #5857, 1.624999999999999778 ) ;
#1149 = CARTESIAN_POINT ( 'NONE',  ( -2.513411990276539942, 1.000000000000000444, -2.949302488239234243 ) ) ;
#1150 = EDGE_CURVE ( 'NONE', #5154, #2549, #2289, .T. ) ;
#1151 = ORIENTED_EDGE ( 'NONE', *, *, #1980, .F. ) ;
#1152 = CARTESIAN_POINT ( 'NONE',  ( -4.462046614173230452, 4.225666661560478765, 8.231249998505111520 ) ) ;
#1153 = DIRECTION ( 'NONE',  ( -0.000000000000000000, -1.000000000000000000, -0.000000000000000000 ) ) ;
#1154 = PERSON_AND_ORGANIZATION_ROLE ( 'creator' ) ;
#1155 = ORIENTED_EDGE ( 'NONE', *, *, #5576, .F. ) ;
#1156 = EDGE_LOOP ( 'NONE', ( #7506, #4920, #4430, #1345 ) ) ;
#1157 = DIRECTION ( 'NONE',  ( -1.000000000000000000, 0.000000000000000000, -0.000000000000000000 ) ) ;
#1158 = CARTESIAN_POINT ( 'NONE',  ( -0.7499999999999993339, 3.950000000000000178, 8.831250000000000711 ) ) ;
#1159 = CARTESIAN_POINT ( 'NONE',  ( 0.000000000000000000, 2.389005866141733492, 4.968462007874015818 ) ) ;
#1160 = ORIENTED_EDGE ( 'NONE', *, *, #5479, .F. ) ;
#1161 = CARTESIAN_POINT ( 'NONE',  ( 3.651126734928074491, 1.000000000000000888, -1.298036420927625167 ) ) ;
#1162 = VERTEX_POINT ( 'NONE', #4160 ) ;
#1163 = EDGE_CURVE ( 'NONE', #6966, #4981, #5316, .T. ) ;
#1164 = PRODUCT_DEFINITION_FORMATION_WITH_SPECIFIED_SOURCE ( 'ANY', '', #1774, .NOT_KNOWN. ) ;
#1165 = CARTESIAN_POINT ( 'NONE',  ( -0.2598750118065171200, 2.345589018234187861, -3.059924881834113819 ) ) ;
#1166 = PRODUCT_RELATED_PRODUCT_CATEGORY ( 'detail', '', ( #3255 ) ) ;
#1167 = DIRECTION ( 'NONE',  ( -0.000000000000000000, -0.000000000000000000, 1.000000000000000000 ) ) ;
#1168 = DIRECTION ( 'NONE',  ( 0.7071067811865474617, 0.000000000000000000, 0.7071067811865474617 ) ) ;
#1169 = CYLINDRICAL_SURFACE ( 'NONE', #5836, 0.3625000000000019318 ) ;
#1170 = ORIENTED_EDGE ( 'NONE', *, *, #4265, .T. ) ;
#1171 = MECHANICAL_CONTEXT ( 'NONE', #5651, 'mechanical' ) ;
#1172 = CARTESIAN_POINT ( 'NONE',  ( -0.7052155605301347885, 5.414000000000000590, 0.5414159055118109576 ) ) ;
#1173 = EDGE_CURVE ( 'NONE', #1938, #5163, #4437, .T. ) ;
#1174 = EDGE_LOOP ( 'NONE', ( #86, #184, #3850, #2849 ) ) ;
#1175 = CARTESIAN_POINT ( 'NONE',  ( 2.537500000000000533, 4.049999999999999822, 0.000000000000000000 ) ) ;
#1176 = CARTESIAN_POINT ( 'NONE',  ( -3.987046614173228587, 3.674333370316265945, 8.231249998505111520 ) ) ;
#1177 = ORIENTED_EDGE ( 'NONE', *, *, #878, .F. ) ;
#1178 = PERSON_AND_ORGANIZATION ( #7862, #8117 ) ;
#1179 = FACE_OUTER_BOUND ( 'NONE', #3877, .T. ) ;
#1180 = COORDINATED_UNIVERSAL_TIME_OFFSET ( 0, 0, .AHEAD. ) ;
#1181 = DIRECTION ( 'NONE',  ( 0.5773502691896257311, -0.5773502691896257311, 0.5773502691896257311 ) ) ;
#1182 = PRODUCT ( 'bench vise2-', 'bench vise2-', '', ( #498 ) ) ;
#1183 = LINE ( 'NONE', #8004, #6979 ) ;
#1184 = CARTESIAN_POINT ( 'NONE',  ( 2.750000000000000888, 8.719000000000001194, 3.813750000000002416 ) ) ;
#1185 = DIRECTION ( 'NONE',  ( 0.000000000000000000, 0.000000000000000000, 1.000000000000000000 ) ) ;
#1186 = VERTEX_POINT ( 'NONE', #6372 ) ;
#1187 = CARTESIAN_POINT ( 'NONE',  ( 1.172489670925565663, 1.365923996832131609E-16, -3.693357951474146361 ) ) ;
#1188 = DIRECTION ( 'NONE',  ( 0.000000000000000000, 0.000000000000000000, -1.000000000000000000 ) ) ;
#1189 = APPROVAL_DATE_TIME ( #3615, #2517 ) ;
#1190 = ORIENTED_EDGE ( 'NONE', *, *, #5387, .F. ) ;
#1191 = DIRECTION ( 'NONE',  ( -0.000000000000000000, -1.000000000000000000, -0.000000000000000000 ) ) ;
#1192 = EDGE_CURVE ( 'NONE', #3226, #6648, #127, .T. ) ;
#1193 = EDGE_CURVE ( 'NONE', #540, #1793, #2196, .T. ) ;
#1194 = ORIENTED_EDGE ( 'NONE', *, *, #249, .F. ) ;
#1195 = LINE ( 'NONE', #6075, #4099 ) ;
#1196 = LINE ( 'NONE', #2959, #2680 ) ;
#1197 = SECURITY_CLASSIFICATION ( '', '', #5602 ) ;
#1198 = ORIENTED_EDGE ( 'NONE', *, *, #6772, .F. ) ;
#1199 = EDGE_LOOP ( 'NONE', ( #834, #3338, #3920, #5891 ) ) ;
#1200 = EDGE_CURVE ( 'NONE', #8086, #4460, #4135, .T. ) ;
#1201 = CARTESIAN_POINT ( 'NONE',  ( -0.4484317010831837536, 2.386788549487817601, -3.019432426063724861 ) ) ;
#1202 = CARTESIAN_POINT ( 'NONE',  ( -1.889618362131626726E-10, 5.414000000000000590, 2.750000000234376074 ) ) ;
#1203 = CARTESIAN_POINT ( 'NONE',  ( 1.187500000000000444, 4.598373714026829262, 6.183596452058795379 ) ) ;
#1204 = ORIENTED_EDGE ( 'NONE', *, *, #3096, .F. ) ;
#1205 = PERSON_AND_ORGANIZATION_ROLE ( 'design_owner' ) ;
#1206 = DIRECTION ( 'NONE',  ( 0.7071067811865474617, -0.000000000000000000, 0.7071067811865474617 ) ) ;
#1207 = CIRCLE ( 'NONE', #6454, 2.619834094488189269 ) ;
#1208 = APPROVAL ( #4500, 'UNSPECIFIED' ) ;
#1209 = CARTESIAN_POINT ( 'NONE',  ( 0.8527717968728635300, 5.380045629463952928, 4.083473622047246288 ) ) ;
#1210 = EDGE_CURVE ( 'NONE', #1295, #2112, #2323, .T. ) ;
#1211 = CARTESIAN_POINT ( 'NONE',  ( -4.066213280839894750, 3.516000035344541530, 7.363250037317452090 ) ) ;
#1212 = ORIENTED_EDGE ( 'NONE', *, *, #7776, .F. ) ;
#1213 = APPROVAL_STATUS ( 'not_yet_approved' ) ;
#1214 = CARTESIAN_POINT ( 'NONE',  ( 0.7335700381840287720, 2.500000000317696536, -5.108750000000001457 ) ) ;
#1215 = DATE_AND_TIME ( #4328, #7635 ) ;
#1216 = CARTESIAN_POINT ( 'NONE',  ( -3.343750000000001776, 2.500000000000000444, -2.750000000000000444 ) ) ;
#1217 = AXIS2_PLACEMENT_3D ( 'NONE', #7608, #6265, #1185 ) ;
#1218 = CIRCLE ( 'NONE', #6193, 0.3625000000000019318 ) ;
#1219 = PLANE ( 'NONE',  #7547 ) ;
#1220 = FACE_OUTER_BOUND ( 'NONE', #1749, .T. ) ;
#1221 = ADVANCED_FACE ( 'NONE', ( #159 ), #6407, .T. ) ;
#1222 = CARTESIAN_POINT ( 'NONE',  ( 1.624999999999999778, 3.950000000000000178, -2.749999999768383940 ) ) ;
#1223 = ORIENTED_EDGE ( 'NONE', *, *, #6059, .F. ) ;
#1224 = CARTESIAN_POINT ( 'NONE',  ( -0.6827599196736721110, 4.260417128052496949, 8.189746072949246170 ) ) ;
#1225 = CARTESIAN_POINT ( 'NONE',  ( 0.000000000000000000, 5.160877715062512472, 6.858307716807694909 ) ) ;
#1226 = ADVANCED_FACE ( 'NONE', ( #913 ), #213, .F. ) ;
#1227 = CIRCLE ( 'NONE', #4488, 0.1875000000000006661 ) ;
#1228 = CALENDAR_DATE ( 2026, 8, 10 ) ;
#1229 = ORIENTED_EDGE ( 'NONE', *, *, #4588, .T. ) ;
#1230 = CIRCLE ( 'NONE', #5669, 2.845000000000001528 ) ;
#1231 = PLANE ( 'NONE',  #6654 ) ;
#1232 = ADVANCED_FACE ( 'NONE', ( #2102 ), #3412, .F. ) ;
#1233 = VECTOR ( 'NONE', #5399, 39.37007874015748854 ) ;
#1234 = EDGE_LOOP ( 'NONE', ( #894, #1547, #2489, #6495, #281, #4071, #6079, #4578 ) ) ;
#1235 = AXIS2_PLACEMENT_3D ( 'NONE', #5040, #7619, #7581 ) ;
#1236 = CARTESIAN_POINT ( 'NONE',  ( 1.500000000000000444, 5.339000000000000412, 0.1249999999999998473 ) ) ;
#1237 = CARTESIAN_POINT ( 'NONE',  ( 0.000000000000000000, 3.950000000000000178, -5.108750000000001457 ) ) ;
#1238 = ORIENTED_EDGE ( 'NONE', *, *, #1082, .F. ) ;
#1239 = CIRCLE ( 'NONE', #2027, 1.074999999999999289 ) ;
#1240 = VERTEX_POINT ( 'NONE', #1490 ) ;
#1241 = ADVANCED_BREP_SHAPE_REPRESENTATION ( '', ( #7800, #7272 ), #588 ) ;
#1242 = SECURITY_CLASSIFICATION ( '', '', #1266 ) ;
#1243 = VECTOR ( 'NONE', #3425, 39.37007874015748143 ) ;
#1244 = DIRECTION ( 'NONE',  ( -0.7071067811865474617, -0.000000000000000000, -0.7071067811865474617 ) ) ;
#1245 = EDGE_CURVE ( 'NONE', #3378, #811, #6496, .T. ) ;
#1246 = AXIS2_PLACEMENT_3D ( 'NONE', #1022, #4823, #2168 ) ;
#1247 = CC_DESIGN_APPROVAL ( #5208, ( #4775 ) ) ;
#1248 = CARTESIAN_POINT ( 'NONE',  ( 0.7631207292863003699, 2.881932780970207109, -5.108750000000001457 ) ) ;
#1249 = AXIS2_PLACEMENT_3D ( 'NONE', #1398, #3436, #856 ) ;
#1250 = CARTESIAN_POINT ( 'NONE',  ( 1.187500000000000666, 4.964596198445718755, 4.572665754078526490 ) ) ;
#1251 = ORIENTED_EDGE ( 'NONE', *, *, #5093, .F. ) ;
#1252 = COORDINATED_UNIVERSAL_TIME_OFFSET ( 0, 0, .AHEAD. ) ;
#1253 = DIRECTION ( 'NONE',  ( 0.9925485533740562305, 0.000000000000000000, 0.1218497812680350845 ) ) ;
#1254 = ORIENTED_EDGE ( 'NONE', *, *, #4966, .F. ) ;
#1255 = VECTOR ( 'NONE', #7754, 39.37007874015748854 ) ;
#1256 = LOCAL_TIME ( 0, 37, 23.00000000000000000, #7348 ) ;
#1257 = CARTESIAN_POINT ( 'NONE',  ( -1.312500000102930775, 4.908106857156239400, 3.316250000000001030 ) ) ;
#1258 = CARTESIAN_POINT ( 'NONE',  ( 0.000000000000000000, 2.875000000000000888, 3.440250000000001140 ) ) ;
#1259 = DIRECTION ( 'NONE',  ( -1.000000000000000000, 0.000000000000000000, -0.000000000000000000 ) ) ;
#1260 = AXIS2_PLACEMENT_3D ( 'NONE', #6807, #3076, #1314 ) ;
#1261 = ORIENTED_EDGE ( 'NONE', *, *, #7159, .F. ) ;
#1262 = AXIS2_PLACEMENT_3D ( 'NONE', #6941, #7714, #2068 ) ;
#1263 = PERSON_AND_ORGANIZATION_ROLE ( 'design_owner' ) ;
#1264 = APPROVAL ( #928, 'UNKNOWN' ) ;
#1265 = CARTESIAN_POINT ( 'NONE',  ( -1.388463899750249738E-31, 3.950000000000000178, -4.043750000000001066 ) ) ;
#1266 = SECURITY_CLASSIFICATION_LEVEL ( 'unclassified' ) ;
#1267 = DIRECTION ( 'NONE',  ( 0.000000000000000000, 0.000000000000000000, -1.000000000000000000 ) ) ;
#1268 = CARTESIAN_POINT ( 'NONE',  ( 2.740000000000000657, 7.964000000000000412, 3.813750000000002416 ) ) ;
#1269 = CIRCLE ( 'NONE', #3865, 0.2625000000000008438 ) ;
#1270 = VECTOR ( 'NONE', #7977, 39.37007874015748143 ) ;
#1271 = CARTESIAN_POINT ( 'NONE',  ( -3.987046614173228587, 3.778630425947245186, 8.135040162507303663 ) ) ;
#1272 = DIRECTION ( 'NONE',  ( -0.000000000000000000, 1.000000000000000000, -0.000000000000000000 ) ) ;
#1273 = DIRECTION ( 'NONE',  ( -7.142086257945775577E-16, -1.000000000000000000, 0.000000000000000000 ) ) ;
#1274 = ORIENTED_EDGE ( 'NONE', *, *, #1891, .F. ) ;
#1275 = CARTESIAN_POINT ( 'NONE',  ( -3.987046614173228587, 3.674333370316265945, 8.231249998505111520 ) ) ;
#1276 = CARTESIAN_POINT ( 'NONE',  ( 0.000000000000000000, 0.000000000000000000, 0.000000000000000000 ) ) ;
#1277 = CC_DESIGN_DATE_AND_TIME_ASSIGNMENT ( #7762, #7682, ( #2137 ) ) ;
#1278 = CARTESIAN_POINT ( 'NONE',  ( -1.187500000000000444, 4.233290553842588899, 6.816515182600094924 ) ) ;
#1279 = AXIS2_PLACEMENT_3D ( 'NONE', #2901, #5393, #2293 ) ;
#1280 = APPROVAL_ROLE ( '' ) ;
#1281 = ORIENTED_EDGE ( 'NONE', *, *, #7096, .F. ) ;
#1282 = CARTESIAN_POINT ( 'NONE',  ( -2.513411990276539942, 1.000000000000000444, -2.949302488239234243 ) ) ;
#1283 = CYLINDRICAL_SURFACE ( 'NONE', #1759, 0.2625000000000008438 ) ;
#1284 = DIRECTION ( 'NONE',  ( 9.769962616696322535E-15, 0.000000000000000000, 1.000000000000000000 ) ) ;
#1285 = ADVANCED_FACE ( 'NONE', ( #6584 ), #259, .T. ) ;
#1286 = VERTEX_POINT ( 'NONE', #3449 ) ;
#1287 = ORIENTED_EDGE ( 'NONE', *, *, #1336, .F. ) ;
#1288 = APPROVAL_PERSON_ORGANIZATION ( #7825, #4358, #2174 ) ;
#1289 = CARTESIAN_POINT ( 'NONE',  ( -3.651126736170069886, 1.365923996832131609E-16, -1.298036422357116138 ) ) ;
#1290 = CARTESIAN_POINT ( 'NONE',  ( 1.310546128896300511, 4.033625775730570240, -5.108750000000004121 ) ) ;
#1291 = CARTESIAN_POINT ( 'NONE',  ( 1.187500000000000444, 4.680108205028392199, 5.951860652718446332 ) ) ;
#1292 = ORIENTED_EDGE ( 'NONE', *, *, #1937, .T. ) ;
#1293 = APPROVAL_STATUS ( 'not_yet_approved' ) ;
#1294 = FACE_OUTER_BOUND ( 'NONE', #4962, .T. ) ;
#1295 = VERTEX_POINT ( 'NONE', #953 ) ;
#1296 = EDGE_CURVE ( 'NONE', #2207, #7215, #6652, .T. ) ;
#1297 = FACE_OUTER_BOUND ( 'NONE', #5302, .T. ) ;
#1298 = CARTESIAN_POINT ( 'NONE',  ( 0.000000000000000000, 5.541000000000003034, 3.956250000000000266 ) ) ;
#1299 = ORIENTED_EDGE ( 'NONE', *, *, #4634, .T. ) ;
#1300 = APPROVAL_STATUS ( 'not_yet_approved' ) ;
#1301 = DIRECTION ( 'NONE',  ( 0.7071067811865474617, 0.000000000000000000, -0.7071067811865474617 ) ) ;
#1302 = CARTESIAN_POINT ( 'NONE',  ( -2.875000000000000888, 1.000000000000000222, -2.975000000000000977 ) ) ;
#1303 =( BOUNDED_SURFACE ( )  B_SPLINE_SURFACE ( 3, 3, ( 
 ( #4178, #383, #3577, #4757 ),
 ( #2353, #4215, #7417, #6735 ),
 ( #1159, #2227, #5521, #4302 ),
 ( #694, #4383, #3769, #5572 ) ),
 .UNSPECIFIED., .F., .F., .T. ) 
 B_SPLINE_SURFACE_WITH_KNOTS ( ( 4, 4 ),
 ( 4, 4 ),
 ( 0.000000000000000000, 1.000000000000000000 ),
 ( 0.000000000000000000, 1.000000000000000000 ),
 .UNSPECIFIED. ) 
 GEOMETRIC_REPRESENTATION_ITEM ( )  RATIONAL_B_SPLINE_SURFACE ( (
 ( 1.000000000000000000, 0.3333333333333330373, 0.3333333333333330373, 1.000000000000000000),
 ( 0.9963935896217739341, 0.3321311965405909783, 0.3321311965405909783, 0.9963935896217739341),
 ( 0.9963935896217739341, 0.3321311965405909783, 0.3321311965405909783, 0.9963935896217739341),
 ( 1.000000000000000000, 0.3333333333333330373, 0.3333333333333330373, 1.000000000000000000) ) ) 
 REPRESENTATION_ITEM ( '' )  SURFACE ( )  );
#1304 = LINE ( 'NONE', #4534, #5856 ) ;
#1305 = CARTESIAN_POINT ( 'NONE',  ( -3.987046614173228587, 3.831386823445361856, 8.074548610981766572 ) ) ;
#1306 = CARTESIAN_POINT ( 'NONE',  ( 1.462953684860233805, 1.000000000000000666, 3.588229579187919960 ) ) ;
#1307 = CARTESIAN_POINT ( 'NONE',  ( -4.382879947506562068, 3.516000035344543306, 8.231249998505111520 ) ) ;
#1308 = EDGE_LOOP ( 'NONE', ( #2995, #1054, #293, #7544 ) ) ;
#1309 = CARTESIAN_POINT ( 'NONE',  ( -2.750000000000000444, 8.574153543168254288, 4.323749999249341336 ) ) ;
#1310 = DIRECTION ( 'NONE',  ( 1.000000000000000000, 0.000000000000000000, 0.000000000000000000 ) ) ;
#1311 = CARTESIAN_POINT ( 'NONE',  ( 2.740000000000001545, 7.964000000000000412, 4.313750000000002416 ) ) ;
#1312 = APPLICATION_PROTOCOL_DEFINITION ( 'international standard', 'config_control_design', 1994, #7793 ) ;
#1313 = EDGE_LOOP ( 'NONE', ( #30, #5281, #881, #8145 ) ) ;
#1314 = DIRECTION ( 'NONE',  ( -1.000000000000000000, 0.000000000000000000, 0.000000000000000000 ) ) ;
#1315 = LOCAL_TIME ( 0, 37, 23.00000000000000000, #4738 ) ;
#1316 = CC_DESIGN_DATE_AND_TIME_ASSIGNMENT ( #2752, #4086, ( #3521 ) ) ;
#1317 = ORGANIZATION ( 'NAUO-ORG12', 'UNSPECIFIED', 'UNSPECIFIED' ) ;
#1318 = CARTESIAN_POINT ( 'NONE',  ( 4.462953385826772035, 4.146499994074615003, 8.231249998505111520 ) ) ;
#1319 = SECURITY_CLASSIFICATION ( '', '', #8135 ) ;
#1320 = CARTESIAN_POINT ( 'NONE',  ( -1.625000000000000222, 0.000000000000000000, 0.1249999999999997641 ) ) ;
#1321 = DIRECTION ( 'NONE',  ( 1.000000000000000000, 0.000000000000000000, 0.000000000000000000 ) ) ;
#1322 = EDGE_CURVE ( 'NONE', #2476, #4355, #6729, .T. ) ;
#1323 = ORIENTED_EDGE ( 'NONE', *, *, #7480, .T. ) ;
#1324 = ORIENTED_EDGE ( 'NONE', *, *, #6787, .F. ) ;
#1325 = CARTESIAN_POINT ( 'NONE',  ( 3.987953385826772834, 4.033008582717783952, 8.053088436265779748 ) ) ;
#1326 = CARTESIAN_POINT ( 'NONE',  ( 0.8990231340611340993, 4.907229921396190520, -5.108749999999997904 ) ) ;
#1327 = EDGE_CURVE ( 'NONE', #941, #5487, #6624, .T. ) ;
#1328 = VERTEX_POINT ( 'NONE', #2837 ) ;
#1329 = LINE ( 'NONE', #1984, #346 ) ;
#1330 = EDGE_CURVE ( 'NONE', #6945, #3927, #4841, .T. ) ;
#1331 = ORIENTED_EDGE ( 'NONE', *, *, #2877, .F. ) ;
#1332 = ADVANCED_FACE ( 'NONE', ( #4797 ), #7774, .T. ) ;
#1333 = FACE_BOUND ( 'NONE', #4286, .T. ) ;
#1334 = CYLINDRICAL_SURFACE ( 'NONE', #4802, 1.624999999999999778 ) ;
#1335 = EDGE_LOOP ( 'NONE', ( #2095, #2588, #6189, #1323, #4194, #2430, #4467, #5777 ) ) ;
#1336 = EDGE_CURVE ( 'NONE', #805, #789, #5448, .T. ) ;
#1337 = PERSON_AND_ORGANIZATION ( #7862, #8117 ) ;
#1338 = DIRECTION ( 'NONE',  ( 0.000000000000000000, -1.000000000000000000, 0.000000000000000000 ) ) ;
#1339 = CARTESIAN_POINT ( 'NONE',  ( -2.740000000000001545, 0.000000000000000000, 4.323750000000001315 ) ) ;
#1340 = CARTESIAN_POINT ( 'NONE',  ( -1.624999999371729231, 2.076218724780642511, 2.750000000000000444 ) ) ;
#1341 = ADVANCED_BREP_SHAPE_REPRESENTATION ( '', ( #7864, #7272 ), #2017 ) ;
#1342 = CARTESIAN_POINT ( 'NONE',  ( 2.875000000000000888, 0.000000000000000000, -3.337500001222715174 ) ) ;
#1343 = DIRECTION ( 'NONE',  ( 0.000000000000000000, 0.000000000000000000, -1.000000000000000000 ) ) ;
#1344 = CARTESIAN_POINT ( 'NONE',  ( -2.537500000000000533, 2.500000000000000444, -0.000000000000000000 ) ) ;
#1345 = ORIENTED_EDGE ( 'NONE', *, *, #162, .F. ) ;
#1346 = CARTESIAN_POINT ( 'NONE',  ( -2.750000000000000444, 7.339000000000003077, 4.175863149606300340 ) ) ;
#1347 = ORIENTED_EDGE ( 'NONE', *, *, #5584, .T. ) ;
#1348 =( NAMED_UNIT ( * ) PLANE_ANGLE_UNIT ( ) SI_UNIT ( $, .RADIAN. ) );
#1349 = CARTESIAN_POINT ( 'NONE',  ( 2.750000000000000444, 7.964000000000000412, 5.236250000000000071 ) ) ;
#1350 = DIRECTION ( 'NONE',  ( -0.000000000000000000, -1.000000000000000000, -0.000000000000000000 ) ) ;
#1351 = DATE_TIME_ROLE ( 'classification_date' ) ;
#1352 = ORIENTED_EDGE ( 'NONE', *, *, #1173, .T. ) ;
#1353 = CARTESIAN_POINT ( 'NONE',  ( 2.740000000000001545, 7.964000000000000412, 4.313750000000002416 ) ) ;
#1354 = VECTOR ( 'NONE', #1898, 39.37007874015748854 ) ;
#1355 = VECTOR ( 'NONE', #5681, 39.37007874015748143 ) ;
#1356 = LOCAL_TIME ( 0, 37, 23.00000000000000000, #3545 ) ;
#1357 = DIRECTION ( 'NONE',  ( 0.000000000000000000, -1.000000000000000000, 0.000000000000000000 ) ) ;
#1358 = CARTESIAN_POINT ( 'NONE',  ( -1.625000000000000222, 2.057992047244095346, -2.750000000000000444 ) ) ;
#1359 = PRODUCT_DEFINITION_SHAPE ( 'NONE', 'NONE',  #8197 ) ;
#1360 = VECTOR ( 'NONE', #1435, 39.37007874015748143 ) ;
#1361 = CARTESIAN_POINT ( 'NONE',  ( -1.625000000000000000, 3.950000000000000178, -2.750000000000000444 ) ) ;
#1362 = DIRECTION ( 'NONE',  ( 1.000000000000000000, 0.000000000000000000, 0.000000000000000000 ) ) ;
#1363 = LOCAL_TIME ( 0, 37, 23.00000000000000000, #2521 ) ;
#1364 = VERTEX_POINT ( 'NONE', #2990 ) ;
#1365 = APPROVAL ( #2053, 'UNSPECIFIED' ) ;
#1366 = VERTEX_POINT ( 'NONE', #4874 ) ;
#1367 = CIRCLE ( 'NONE', #32, 3.000000000000001332 ) ;
#1368 = DESIGN_CONTEXT ( 'detailed design', #4603, 'design' ) ;
#1369 = CIRCLE ( 'NONE', #3841, 2.999999999836793663 ) ;
#1370 = AXIS2_PLACEMENT_3D ( 'NONE', #369, #7140, #3528 ) ;
#1371 = CARTESIAN_POINT ( 'NONE',  ( 3.987953385826772834, 3.820636894297861019, 8.082722253683524372 ) ) ;
#1372 = CARTESIAN_POINT ( 'NONE',  ( 0.7977802186893850900, 2.907566522260822239, -5.108750000000001457 ) ) ;
#1373 = DIRECTION ( 'NONE',  ( 0.000000000000000000, 0.000000000000000000, -1.000000000000000000 ) ) ;
#1374 = VECTOR ( 'NONE', #5430, 39.37007874015748143 ) ;
#1375 = APPROVAL ( #3511, 'UNSPECIFIED' ) ;
#1376 = CARTESIAN_POINT ( 'NONE',  ( 0.000000000000000000, 3.950000000000000178, 3.316250000000001030 ) ) ;
#1377 = ORIENTED_EDGE ( 'NONE', *, *, #7885, .F. ) ;
#1378 = VECTOR ( 'NONE', #7948, 39.37007874015748854 ) ;
#1379 = VECTOR ( 'NONE', #2329, 39.37007874015748143 ) ;
#1380 =( GEOMETRIC_REPRESENTATION_CONTEXT ( 3 ) GLOBAL_UNCERTAINTY_ASSIGNED_CONTEXT ( ( #6450 ) ) GLOBAL_UNIT_ASSIGNED_CONTEXT ( ( #7737, #4617, #2125 ) ) REPRESENTATION_CONTEXT ( 'NONE', 'WORKASPACE' ) );
#1381 = EDGE_CURVE ( 'NONE', #4517, #3043, #6117, .T. ) ;
#1382 = FACE_OUTER_BOUND ( 'NONE', #6122, .T. ) ;
#1383 = CARTESIAN_POINT ( 'NONE',  ( 0.000000000000000000, 5.151388682096968097, -2.750000000000000444 ) ) ;
#1384 = ORIENTED_EDGE ( 'NONE', *, *, #8012, .F. ) ;
#1385 = PERSON_AND_ORGANIZATION_ROLE ( 'creator' ) ;
#1386 = EDGE_CURVE ( 'NONE', #2452, #5045, #3496, .T. ) ;
#1387 = PLANE ( 'NONE',  #7970 ) ;
#1388 = PERSON_AND_ORGANIZATION ( #4965, #7699 ) ;
#1389 = VECTOR ( 'NONE', #3934, 39.37007874015748143 ) ;
#1390 = EDGE_LOOP ( 'NONE', ( #3054, #7873, #5510, #5186 ) ) ;
#1391 = CARTESIAN_POINT ( 'NONE',  ( 0.000000000000000000, 7.521783346469146814, 3.956249999985041566 ) ) ;
#1392 = CARTESIAN_POINT ( 'NONE',  ( 0.000000000000000000, 5.536672282146935409, 4.083473622047245399 ) ) ;
#1393 = AXIS2_PLACEMENT_3D ( 'NONE', #464, #5911, #5409 ) ;
#1394 = CARTESIAN_POINT ( 'NONE',  ( -3.987046614173229475, 3.853790179936717575, 8.402619588493877245 ) ) ;
#1395 = ORIENTED_EDGE ( 'NONE', *, *, #1296, .F. ) ;
#1396 = CARTESIAN_POINT ( 'NONE',  ( -2.750000000000000444, 7.339000000000003077, 5.236250000000000071 ) ) ;
#1397 = ORIENTED_EDGE ( 'NONE', *, *, #1873, .F. ) ;
#1398 = CARTESIAN_POINT ( 'NONE',  ( 1.405994097256312081, 2.812660052342375927, 6.777379598874453848 ) ) ;
#1399 = CARTESIAN_POINT ( 'NONE',  ( 2.750000000000000444, 7.541160346212514298, 3.932968645167688404 ) ) ;
#1400 = CARTESIAN_POINT ( 'NONE',  ( 3.484120143574221651E-16, 1.750000000000000444, 2.845000000000001528 ) ) ;
#1401 = PERSON_AND_ORGANIZATION_ROLE ( 'creator' ) ;
#1402 = ORIENTED_EDGE ( 'NONE', *, *, #6970, .T. ) ;
#1403 = FACE_OUTER_BOUND ( 'NONE', #341, .T. ) ;
#1404 = AXIS2_PLACEMENT_3D ( 'NONE', #5188, #2737, #7005 ) ;
#1405 = CYLINDRICAL_SURFACE ( 'NONE', #2679, 1.624999999999999778 ) ;
#1406 = CIRCLE ( 'NONE', #6769, 0.4312500000000004663 ) ;
#1407 = AXIS2_PLACEMENT_3D ( 'NONE', #6609, #1754, #986 ) ;
#1408 = CARTESIAN_POINT ( 'NONE',  ( 0.000000000000000000, 3.950000000000000178, 7.231250000000000178 ) ) ;
#1409 = ORIENTED_EDGE ( 'NONE', *, *, #6886, .F. ) ;
#1410 = EDGE_CURVE ( 'NONE', #1993, #3049, #5415, .T. ) ;
#1411 = CARTESIAN_POINT ( 'NONE',  ( -0.7210596466522595227, 3.743128570366073937, 7.996158673814918849 ) ) ;
#1412 = CARTESIAN_POINT ( 'NONE',  ( 0.7386972477860229702, 3.819935838229653768, 8.515578956946562528 ) ) ;
#1413 = ORIENTED_EDGE ( 'NONE', *, *, #4346, .F. ) ;
#1414 = CARTESIAN_POINT ( 'NONE',  ( 3.987953385826771946, 3.771838453699690508, 8.148241431725164574 ) ) ;
#1415 = CARTESIAN_POINT ( 'NONE',  ( 0.2965954892784562480, 2.670736509751080678, -5.108749999999998792 ) ) ;
#1416 = CARTESIAN_POINT ( 'NONE',  ( 3.987953385826772390, 3.856588441155107017, 8.404352163763244121 ) ) ;
#1417 = CARTESIAN_POINT ( 'NONE',  ( 1.347488133127687560, 2.365290551318774082, 2.749999999536767437 ) ) ;
#1418 = ORIENTED_EDGE ( 'NONE', *, *, #8044, .T. ) ;
#1419 = PRODUCT_DEFINITION ( 'UNKNOWN', '', #6576, #7966 ) ;
#1420 = APPROVAL_PERSON_ORGANIZATION ( #3155, #4565, #7497 ) ;
#1421 = CYLINDRICAL_SURFACE ( 'NONE', #2304, 0.3625000000000019318 ) ;
#1422 = CARTESIAN_POINT ( 'NONE',  ( 2.150000000000000799, 2.875000000000000888, 3.440250000000000696 ) ) ;
#1423 = ORIENTED_EDGE ( 'NONE', *, *, #4838, .T. ) ;
#1424 = APPROVAL_ROLE ( '' ) ;
#1425 = FACE_OUTER_BOUND ( 'NONE', #3014, .T. ) ;
#1426 = EDGE_CURVE ( 'NONE', #6692, #6736, #4174, .T. ) ;
#1427 = EDGE_CURVE ( 'NONE', #7586, #445, #1650, .T. ) ;
#1428 = APPROVAL_DATE_TIME ( #2654, #1264 ) ;
#1429 = CARTESIAN_POINT ( 'NONE',  ( 0.7466433925744948574, 3.878406391858416402, 7.926888364618726257 ) ) ;
#1430 = CARTESIAN_POINT ( 'NONE',  ( 1.172489670925564997, 1.365923996832131609E-16, -3.693357951474146805 ) ) ;
#1431 = FACE_OUTER_BOUND ( 'NONE', #3309, .T. ) ;
#1432 = PRODUCT ( 'bench vise6-', 'bench vise6-', '', ( #4190 ) ) ;
#1433 = ADVANCED_FACE ( 'NONE', ( #4997 ), #8137, .F. ) ;
#1434 = VERTEX_POINT ( 'NONE', #7578 ) ;
#1435 = DIRECTION ( 'NONE',  ( 0.000000000000000000, 1.000000000000000000, 0.000000000000000000 ) ) ;
#1436 = CARTESIAN_POINT ( 'NONE',  ( -3.987046614173228587, 4.146499994074616779, 8.231249998505111520 ) ) ;
#1437 = EDGE_LOOP ( 'NONE', ( #4155, #4340, #3099, #7213 ) ) ;
#1438 = CARTESIAN_POINT ( 'NONE',  ( -4.066213280839894750, 3.516000035344541530, 9.099249959692773615 ) ) ;
#1439 = DIRECTION ( 'NONE',  ( -0.2747029802028605472, 0.000000000000000000, 0.9615291325111615661 ) ) ;
#1440 = CARTESIAN_POINT ( 'NONE',  ( -2.750000000000000444, 7.964000000000000412, 5.236250000000000071 ) ) ;
#1441 = PERSON_AND_ORGANIZATION_ROLE ( 'classification_officer' ) ;
#1442 = VERTEX_POINT ( 'NONE', #2474 ) ;
#1443 = CARTESIAN_POINT ( 'NONE',  ( -4.462046614173229564, 3.753500037801645206, 8.624249954778562710 ) ) ;
#1444 = CARTESIAN_POINT ( 'NONE',  ( 2.750000000000000444, 8.589000000000000412, 3.161250000000001670 ) ) ;
#1445 = CARTESIAN_POINT ( 'NONE',  ( 2.750000000000000444, 7.973999999999999311, 4.313750000000002416 ) ) ;
#1446 = DATE_AND_TIME ( #3745, #3707 ) ;
#1447 = ADVANCED_FACE ( 'NONE', ( #6930 ), #1929, .F. ) ;
#1448 = ORIENTED_EDGE ( 'NONE', *, *, #2784, .T. ) ;
#1449 = CARTESIAN_POINT ( 'NONE',  ( -0.7386972477860230812, 3.819935838229653768, 7.946921043053440492 ) ) ;
#1450 = EDGE_LOOP ( 'NONE', ( #5896, #6287, #119, #4407 ) ) ;
#1451 = UNCERTAINTY_MEASURE_WITH_UNIT (LENGTH_MEASURE( 1.000000000000000082E-05 ), #3612, 'distance_accuracy_value', 'NONE');
#1452 = CARTESIAN_POINT ( 'NONE',  ( 3.987953385826772390, 3.793298628413402263, 8.112636806013968638 ) ) ;
#1453 = CARTESIAN_POINT ( 'NONE',  ( -3.362500000000001155, 1.750000000000000444, 4.117874862132976456E-16 ) ) ;
#1454 = ADVANCED_FACE ( 'NONE', ( #4423 ), #3773, .T. ) ;
#1455 = CARTESIAN_POINT ( 'NONE',  ( 3.987953385826772834, 3.900888680988107371, 8.423148454254921091 ) ) ;
#1456 = VERTEX_POINT ( 'NONE', #5038 ) ;
#1457 = CARTESIAN_POINT ( 'NONE',  ( -3.791570908345035740, 1.000000000000000222, 0.7997593681799639587 ) ) ;
#1458 = DIRECTION ( 'NONE',  ( 0.000000000000000000, 0.000000000000000000, -1.000000000000000000 ) ) ;
#1459 = CARTESIAN_POINT ( 'NONE',  ( 3.343750000000001776, 0.000000000000000000, 0.000000000000000000 ) ) ;
#1460 = ORIENTED_EDGE ( 'NONE', *, *, #4983, .F. ) ;
#1461 = PERSON_AND_ORGANIZATION_ROLE ( 'design_supplier' ) ;
#1462 = DIRECTION ( 'NONE',  ( 0.000000000000000000, 0.000000000000000000, 1.000000000000000000 ) ) ;
#1463 = ITEM_DEFINED_TRANSFORMATION ( 'NONE', 'NONE', #7567,  #7272 ) ;
#1464 = CARTESIAN_POINT ( 'NONE',  ( 0.6866307324975363668, 3.648256581353261030, 8.149316802294766404 ) ) ;
#1465 = PRODUCT_RELATED_PRODUCT_CATEGORY ( 'detail', '', ( #6809 ) ) ;
#1466 = CARTESIAN_POINT ( 'NONE',  ( 3.987953385826772390, 3.753500037802128375, 8.231249998505111520 ) ) ;
#1467 =( BOUNDED_CURVE ( )  B_SPLINE_CURVE ( 3, ( #1453, #3930, #1654, #4177 ),
 .UNSPECIFIED., .F., .F. ) 
 B_SPLINE_CURVE_WITH_KNOTS ( ( 4, 4 ),
 ( 0.000000000000000000, 0.2669680800879516980 ),
 .UNSPECIFIED. ) 
 CURVE ( )  GEOMETRIC_REPRESENTATION_ITEM ( )  RATIONAL_B_SPLINE_CURVE ( ( 1.000000000000000000, 0.3333333333333334259, 0.3333333333333334259, 1.000000000000000000 ) ) 
 REPRESENTATION_ITEM ( '' )  );
#1468 = EDGE_CURVE ( 'NONE', #1711, #295, #4959, .T. ) ;
#1469 = VERTEX_POINT ( 'NONE', #5575 ) ;
#1470 = EDGE_CURVE ( 'NONE', #3236, #1962, #5866, .T. ) ;
#1471 = CARTESIAN_POINT ( 'NONE',  ( -3.987046614173228587, 4.060302611091305636, 8.393904357314925235 ) ) ;
#1472 = ORIENTED_EDGE ( 'NONE', *, *, #1085, .T. ) ;
#1473 = CARTESIAN_POINT ( 'NONE',  ( -1.187500000000000000, 8.523567361455139491, 4.820336051656679999 ) ) ;
#1474 = ORIENTED_EDGE ( 'NONE', *, *, #3382, .T. ) ;
#1475 = CARTESIAN_POINT ( 'NONE',  ( -1.187500000000000000, 4.964569481811528462, 4.572968553284305848 ) ) ;
#1476 = COORDINATED_UNIVERSAL_TIME_OFFSET ( 0, 0, .AHEAD. ) ;
#1477 = VERTEX_POINT ( 'NONE', #623 ) ;
#1478 = CARTESIAN_POINT ( 'NONE',  ( -0.3427224271551993495, 2.680139432305034930, -5.108749999999998792 ) ) ;
#1479 = EDGE_CURVE ( 'NONE', #5688, #5130, #3157, .T. ) ;
#1480 = LINE ( 'NONE', #5320, #3329 ) ;
#1481 = CARTESIAN_POINT ( 'NONE',  ( -2.750000000000000444, 7.339000000000003077, 2.411250000000000338 ) ) ;
#1482 = SHAPE_REPRESENTATION_RELATIONSHIP ( 'NONE' , 'NONE' ,  #4229, #1341 ) ;
#1483 = CARTESIAN_POINT ( 'NONE',  ( 0.7052155605301347885, 5.414000000000000590, 0.1249999999999999029 ) ) ;
#1484 = ORIENTED_EDGE ( 'NONE', *, *, #2339, .F. ) ;
#1485 = AXIS2_PLACEMENT_3D ( 'NONE', #690, #4950, #1839 ) ;
#1486 = COORDINATED_UNIVERSAL_TIME_OFFSET ( 0, 0, .AHEAD. ) ;
#1487 = ORIENTED_EDGE ( 'NONE', *, *, #2898, .F. ) ;
#1488 = AXIS2_PLACEMENT_3D ( 'NONE', #1760, #4790, #7955 ) ;
#1489 = EDGE_CURVE ( 'NONE', #5456, #2413, #468, .T. ) ;
#1490 = CARTESIAN_POINT ( 'NONE',  ( -3.343750000000002220, 1.749999999935557327, 0.5625000000000003331 ) ) ;
#1491 = PRODUCT_DEFINITION_FORMATION_WITH_SPECIFIED_SOURCE ( 'ANY', '', #5212, .NOT_KNOWN. ) ;
#1492 = CARTESIAN_POINT ( 'NONE',  ( 0.6863513793485908066, 3.647607376475762830, 8.312718817107960234 ) ) ;
#1493 = AXIS2_PLACEMENT_3D ( 'NONE', #1652, #5285, #4754 ) ;
#1494 = CC_DESIGN_APPROVAL ( #1375, ( #303 ) ) ;
#1495 = CARTESIAN_POINT ( 'NONE',  ( 3.987953385826771058, 3.789313681611198970, 8.118096427186111796 ) ) ;
#1496 = CARTESIAN_POINT ( 'NONE',  ( 4.462953385826771147, 3.753500037802127931, 8.231249998505111520 ) ) ;
#1497 = CARTESIAN_POINT ( 'NONE',  ( -2.750000000000000444, 8.719000000000002970, 3.833750000000001545 ) ) ;
#1498 = EDGE_LOOP ( 'NONE', ( #3162, #4098, #6279, #5676 ) ) ;
#1499 = CARTESIAN_POINT ( 'NONE',  ( 2.750000000000000444, 8.601278779527561369, 3.956250000127937483 ) ) ;
#1500 = VERTEX_POINT ( 'NONE', #534 ) ;
#1501 = VECTOR ( 'NONE', #692, 39.37007874015748143 ) ;
#1502 = ADVANCED_FACE ( 'NONE', ( #6315 ), #1231, .T. ) ;
#1503 = DIRECTION ( 'NONE',  ( 0.000000000000000000, 0.000000000000000000, 1.000000000000000000 ) ) ;
#1504 = VECTOR ( 'NONE', #133, 39.37007874015748143 ) ;
#1505 = VECTOR ( 'NONE', #627, 39.37007874015748143 ) ;
#1506 = PLANE ( 'NONE',  #6080 ) ;
#1507 = VERTEX_POINT ( 'NONE', #3199 ) ;
#1508 = CALENDAR_DATE ( 2026, 8, 10 ) ;
#1509 = DIRECTION ( 'NONE',  ( -1.000000000000000000, 0.000000000000000000, 0.000000000000000000 ) ) ;
#1510 = DIRECTION ( 'NONE',  ( -0.000000000000000000, -1.000000000000000000, -0.000000000000000000 ) ) ;
#1511 = CARTESIAN_POINT ( 'NONE',  ( 0.7431911064911158604, 4.051321384912569101, 8.527048809074747382 ) ) ;
#1512 = VECTOR ( 'NONE', #5979, 39.37007874015748143 ) ;
#1513 =( GEOMETRIC_REPRESENTATION_CONTEXT ( 3 ) GLOBAL_UNCERTAINTY_ASSIGNED_CONTEXT ( ( #1612 ) ) GLOBAL_UNIT_ASSIGNED_CONTEXT ( ( #4457, #1348, #3838 ) ) REPRESENTATION_CONTEXT ( 'NONE', 'WORKASPACE' ) );
#1514 = ORIENTED_EDGE ( 'NONE', *, *, #7488, .T. ) ;
#1515 = DIRECTION ( 'NONE',  ( 0.1218497814115311745, 0.000000000000000000, 0.9925485533564400997 ) ) ;
#1516 = CARTESIAN_POINT ( 'NONE',  ( -3.987046614173228587, 3.879123177173203540, 8.414523909741193464 ) ) ;
#1517 = ORIENTED_EDGE ( 'NONE', *, *, #7885, .T. ) ;
#1518 = DIRECTION ( 'NONE',  ( 0.000000000000000000, 0.7071067811865475727, 0.7071067811865475727 ) ) ;
#1519 = DIRECTION ( 'NONE',  ( 0.000000000000000000, 0.000000000000000000, 1.000000000000000000 ) ) ;
#1520 = DIRECTION ( 'NONE',  ( 0.5773502691896257311, 0.5773502691896257311, -0.5773502691896257311 ) ) ;
#1521 = APPROVAL_PERSON_ORGANIZATION ( #6049, #6489, #6706 ) ;
#1522 = CALENDAR_DATE ( 2026, 8, 10 ) ;
#1523 = EDGE_CURVE ( 'NONE', #6692, #5123, #3124, .T. ) ;
#1524 = ORIENTED_EDGE ( 'NONE', *, *, #6938, .T. ) ;
#1525 = AXIS2_PLACEMENT_3D ( 'NONE', #4566, #3863, #3341 ) ;
#1526 = DIRECTION ( 'NONE',  ( -0.000000000000000000, 1.000000000000000000, -0.000000000000000000 ) ) ;
#1527 = CC_DESIGN_PERSON_AND_ORGANIZATION_ASSIGNMENT ( #135, #2652, ( #4564 ) ) ;
#1528 = CARTESIAN_POINT ( 'NONE',  ( -1.201750196850394081, 2.500000000000000444, -2.750000000000000444 ) ) ;
#1529 = CARTESIAN_POINT ( 'NONE',  ( -2.875000000000000888, 0.000000000000000000, -2.975000000000000977 ) ) ;
#1530 = ORIENTED_EDGE ( 'NONE', *, *, #4992, .F. ) ;
#1531 = COORDINATED_UNIVERSAL_TIME_OFFSET ( 0, 0, .AHEAD. ) ;
#1532 = APPLICATION_CONTEXT ( 'configuration controlled 3d designs of mechanical parts and assemblies' ) ;
#1533 = VERTEX_POINT ( 'NONE', #5696 ) ;
#1534 = DIRECTION ( 'NONE',  ( 0.000000000000000000, -0.000000000000000000, 1.000000000000000000 ) ) ;
#1535 = CARTESIAN_POINT ( 'NONE',  ( 0.7370170160409607041, 3.810752038529029218, 8.511197325751680864 ) ) ;
#1536 = ADVANCED_FACE ( 'NONE', ( #71 ), #8094, .T. ) ;
#1537 = AXIS2_PLACEMENT_3D ( 'NONE', #5300, #848, #2204 ) ;
#1538 = EDGE_CURVE ( 'NONE', #4491, #1578, #5591, .T. ) ;
#1539 = DIRECTION ( 'NONE',  ( 0.000000000000000000, 0.000000000000000000, 1.000000000000000000 ) ) ;
#1540 = PLANE ( 'NONE',  #3451 ) ;
#1541 = CARTESIAN_POINT ( 'NONE',  ( 3.987953385826772390, 4.123102181194456151, 8.324661573291658456 ) ) ;
#1542 = ORIENTED_EDGE ( 'NONE', *, *, #3875, .F. ) ;
#1543 = VECTOR ( 'NONE', #5875, 39.37007874015748143 ) ;
#1544 = CARTESIAN_POINT ( 'NONE',  ( 1.274606805570081214, 2.434036455782362829, -2.749999999536767437 ) ) ;
#1545 = AXIS2_PLACEMENT_3D ( 'NONE', #5081, #3845, #3805 ) ;
#1546 = DIRECTION ( 'NONE',  ( 0.000000000000000000, -1.000000000000000000, 0.000000000000000000 ) ) ;
#1547 = ORIENTED_EDGE ( 'NONE', *, *, #4549, .F. ) ;
#1548 = COORDINATED_UNIVERSAL_TIME_OFFSET ( 0, 0, .AHEAD. ) ;
#1549 = LINE ( 'NONE', #4030, #6499 ) ;
#1550 = EDGE_CURVE ( 'NONE', #8018, #7102, #6186, .T. ) ;
#1551 = PERSON_AND_ORGANIZATION ( #5168, #660 ) ;
#1552 = CYLINDRICAL_SURFACE ( 'NONE', #4481, 0.3625000000000019318 ) ;
#1553 = FACE_OUTER_BOUND ( 'NONE', #6757, .T. ) ;
#1554 = ORIENTED_EDGE ( 'NONE', *, *, #7424, .T. ) ;
#1555 = CARTESIAN_POINT ( 'NONE',  ( -3.987046614173228587, 3.848075132173495394, 8.399281692864384752 ) ) ;
#1556 = DIRECTION ( 'NONE',  ( 0.000000000000000000, -0.000000000000000000, -1.000000000000000000 ) ) ;
#1557 = CARTESIAN_POINT ( 'NONE',  ( -3.796513189164424151, 1.365923996832131609E-16, -2.946478859991638277 ) ) ;
#1558 = ORIENTED_EDGE ( 'NONE', *, *, #1077, .T. ) ;
#1559 = CARTESIAN_POINT ( 'NONE',  ( -3.571105955780006891, 2.812660052342378592, 6.581740305714693484 ) ) ;
#1560 = DIRECTION ( 'NONE',  ( 0.000000000000000000, 0.000000000000000000, -1.000000000000000000 ) ) ;
#1561 = CALENDAR_DATE ( 2026, 8, 10 ) ;
#1562 = ORIENTED_EDGE ( 'NONE', *, *, #3394, .F. ) ;
#1563 = CARTESIAN_POINT ( 'NONE',  ( 0.001186118861278498285, 5.262499470843738258, -5.108750000000001457 ) ) ;
#1564 = CARTESIAN_POINT ( 'NONE',  ( -1.136188160962484872, 4.607419020399388110, -5.108750000000003233 ) ) ;
#1565 = CARTESIAN_POINT ( 'NONE',  ( 1.249999999999999556, 3.950000000000000178, -4.308749999765625560 ) ) ;
#1566 = DIRECTION ( 'NONE',  ( 0.000000000000000000, 0.000000000000000000, -1.000000000000000000 ) ) ;
#1567 = PERSON_AND_ORGANIZATION ( #7862, #8117 ) ;
#1568 = PERSON ( 'NAUO-PER6', 'UNSPECIFIED', 'UNSPECIFIED', ('UNSPECIFIED'), ('UNSPECIFIED'), ('UNSPECIFIED') ) ;
#1569 = ORIENTED_EDGE ( 'NONE', *, *, #1779, .T. ) ;
#1570 = DIRECTION ( 'NONE',  ( 0.000000000000000000, 1.000000000000000000, 0.000000000000000000 ) ) ;
#1571 = CC_DESIGN_PERSON_AND_ORGANIZATION_ASSIGNMENT ( #2988, #6965, ( #1182 ) ) ;
#1572 = ADVANCED_FACE ( 'NONE', ( #1814 ), #575, .F. ) ;
#1573 = CARTESIAN_POINT ( 'NONE',  ( 2.750000000000000888, 7.974000000000001087, 3.823750000000002647 ) ) ;
#1574 = CARTESIAN_POINT ( 'NONE',  ( 3.987953385826771946, 3.753500037802127931, 8.231249998505111520 ) ) ;
#1575 = CARTESIAN_POINT ( 'NONE',  ( -3.484361157709182422, 0.9999999999998147038, -1.767115912624255047 ) ) ;
#1576 = CARTESIAN_POINT ( 'NONE',  ( 3.987953385826772390, 4.146499994074615003, 8.231249998505111520 ) ) ;
#1577 = CARTESIAN_POINT ( 'NONE',  ( -0.7122963468828453770, 3.714722057770372121, 8.437904003344627313 ) ) ;
#1578 = VERTEX_POINT ( 'NONE', #8181 ) ;
#1579 = SECURITY_CLASSIFICATION ( '', '', #5513 ) ;
#1580 = LINE ( 'NONE', #4060, #2530 ) ;
#1581 = EDGE_CURVE ( 'NONE', #2711, #4311, #6967, .T. ) ;
#1582 = CARTESIAN_POINT ( 'NONE',  ( 1.625000000000000222, 5.339000000000000412, -2.750000000000000444 ) ) ;
#1583 = DIRECTION ( 'NONE',  ( 0.000000000000000000, 0.000000000000000000, 1.000000000000000000 ) ) ;
#1584 = EDGE_CURVE ( 'NONE', #8024, #3627, #3237, .T. ) ;
#1585 = ADVANCED_FACE ( 'NONE', ( #1403 ), #6359, .F. ) ;
#1586 = CARTESIAN_POINT ( 'NONE',  ( 0.1311681248375602682, 2.329016406037186737, -3.076246856427637510 ) ) ;
#1587 = CARTESIAN_POINT ( 'NONE',  ( -2.740000000000001545, 7.964000000000000412, 3.833750000000001545 ) ) ;
#1588 = ORIENTED_EDGE ( 'NONE', *, *, #735, .F. ) ;
#1589 = APPROVAL_PERSON_ORGANIZATION ( #6770, #7758, #6726 ) ;
#1590 = PERSON_AND_ORGANIZATION_ROLE ( 'creator' ) ;
#1591 = CARTESIAN_POINT ( 'NONE',  ( -0.7052155605301346775, 5.414000000000000590, 0.000000000000000000 ) ) ;
#1592 = PERSON_AND_ORGANIZATION ( #7112, #6095 ) ;
#1593 = CARTESIAN_POINT ( 'NONE',  ( 0.6836440906233618442, 4.258440652362253331, 8.180003846963320058 ) ) ;
#1594 = CARTESIAN_POINT ( 'NONE',  ( 2.750000000000000888, 8.729000000000002757, 3.333750000000001990 ) ) ;
#1595 = ADVANCED_FACE ( 'NONE', ( #5742 ), #1303, .T. ) ;
#1596 = ORIENTED_EDGE ( 'NONE', *, *, #228, .F. ) ;
#1597 = EDGE_CURVE ( 'NONE', #6568, #3656, #2507, .T. ) ;
#1598 = CARTESIAN_POINT ( 'NONE',  ( 1.625000000000000222, 5.113999999999999879, 2.750000000000000444 ) ) ;
#1599 = LINE ( 'NONE', #6607, #1379 ) ;
#1600 = LINE ( 'NONE', #4579, #3335 ) ;
#1601 = VERTEX_POINT ( 'NONE', #7496 ) ;
#1602 = DIRECTION ( 'NONE',  ( -0.000000000000000000, 1.000000000000000000, -0.000000000000000000 ) ) ;
#1603 = PERSON_AND_ORGANIZATION ( #7862, #8117 ) ;
#1604 = ORIENTED_EDGE ( 'NONE', *, *, #1192, .T. ) ;
#1605 = CARTESIAN_POINT ( 'NONE',  ( -0.7665824524342863544, 2.883775449096970256, -5.108750000000003233 ) ) ;
#1606 = EDGE_CURVE ( 'NONE', #5196, #8146, #7404, .T. ) ;
#1607 = CARTESIAN_POINT ( 'NONE',  ( 0.08076397176416273693, 2.326924981622356281, 3.078310609319442115 ) ) ;
#1608 = CARTESIAN_POINT ( 'NONE',  ( -2.750000000000000444, 7.964000000000000412, 3.833750000000001545 ) ) ;
#1609 = CARTESIAN_POINT ( 'NONE',  ( -3.762484563843160768, 1.281112611882646579, 7.524969127686321535 ) ) ;
#1610 = CALENDAR_DATE ( 2026, 8, 10 ) ;
#1611 = ORIENTED_EDGE ( 'NONE', *, *, #5286, .F. ) ;
#1612 = UNCERTAINTY_MEASURE_WITH_UNIT (LENGTH_MEASURE( 1.000000000000000082E-05 ), #4457, 'distance_accuracy_value', 'NONE');
#1613 = DIRECTION ( 'NONE',  ( -1.000000000000000000, 0.000000000000000000, 0.000000000000000000 ) ) ;
#1614 = APPROVAL ( #5436, 'UNKNOWN' ) ;
#1615 = DIRECTION ( 'NONE',  ( 0.7071067811865474617, 0.000000000000000000, 0.7071067811865474617 ) ) ;
#1616 = CARTESIAN_POINT ( 'NONE',  ( 3.987953385826771946, 4.118100097281283567, 8.333224921929698326 ) ) ;
#1617 = ORIENTED_EDGE ( 'NONE', *, *, #2536, .F. ) ;
#1618 = VECTOR ( 'NONE', #5923, 39.37007874015748143 ) ;
#1619 = CC_DESIGN_SECURITY_CLASSIFICATION ( #4483, ( #5941 ) ) ;
#1620 = DIRECTION ( 'NONE',  ( 1.000000000000000000, 0.000000000000000000, -1.986798540846736797E-16 ) ) ;
#1621 = CARTESIAN_POINT ( 'NONE',  ( -3.343750000000001776, 1.750000000000000444, -0.5625000000000003331 ) ) ;
#1622 = PRODUCT_DEFINITION ( 'UNKNOWN', '', #4741, #378 ) ;
#1623 = LINE ( 'NONE', #5500, #3959 ) ;
#1624 = ORIENTED_EDGE ( 'NONE', *, *, #7047, .F. ) ;
#1625 = PERSON_AND_ORGANIZATION ( #7862, #8117 ) ;
#1626 = AXIS2_PLACEMENT_3D ( 'NONE', #7841, #4803, #2258 ) ;
#1627 = DIRECTION ( 'NONE',  ( 0.000000000000000000, 1.000000000000000000, 0.000000000000000000 ) ) ;
#1628 = DIRECTION ( 'NONE',  ( 0.000000000000000000, 1.000000000000000000, 0.000000000000000000 ) ) ;
#1629 = LOCAL_TIME ( 0, 37, 23.00000000000000000, #5829 ) ;
#1630 = CARTESIAN_POINT ( 'NONE',  ( 0.6889980206436411292, 4.246403994982890673, 8.130130038714289853 ) ) ;
#1631 = CONICAL_SURFACE ( 'NONE', #5024, 0.7499999999999993339, 0.7853981633974437271 ) ;
#1632 = VERTEX_POINT ( 'NONE', #6842 ) ;
#1633 = ADVANCED_FACE ( 'N', ( #5611 ), #4994, .T. ) ;
#1634 = ORIENTED_EDGE ( 'NONE', *, *, #7668, .F. ) ;
#1635 = DIRECTION ( 'NONE',  ( 0.000000000000000000, 1.000000000000000000, 0.000000000000000000 ) ) ;
#1636 = ORIENTED_EDGE ( 'NONE', *, *, #562, .T. ) ;
#1637 = PERSON_AND_ORGANIZATION ( #7862, #8117 ) ;
#1638 = CARTESIAN_POINT ( 'NONE',  ( -0.7335700375402988138, 2.499999999992026378, 2.908930215739981229 ) ) ;
#1639 = VECTOR ( 'NONE', #4243, 39.37007874015748143 ) ;
#1640 = ORIENTED_EDGE ( 'NONE', *, *, #3371, .F. ) ;
#1641 = CARTESIAN_POINT ( 'NONE',  ( -1.624999999560674535, 2.217843349570411515, 2.674602988970680606 ) ) ;
#1642 = EDGE_CURVE ( 'NONE', #3433, #5914, #5864, .T. ) ;
#1643 = FACE_OUTER_BOUND ( 'NONE', #7950, .T. ) ;
#1644 = AXIS2_PLACEMENT_3D ( 'NONE', #399, #2892, #1556 ) ;
#1645 = APPROVAL_PERSON_ORGANIZATION ( #1388, #3415, #4368 ) ;
#1646 = CARTESIAN_POINT ( 'NONE',  ( -1.624999999999998446, 5.151388682096968097, 2.750000000000000444 ) ) ;
#1647 = CARTESIAN_POINT ( 'NONE',  ( 1.074999999999999289, 3.950000000000000178, -4.043750000000001066 ) ) ;
#1648 = CALENDAR_DATE ( 2026, 8, 10 ) ;
#1649 = ORIENTED_EDGE ( 'NONE', *, *, #6889, .T. ) ;
#1650 = LINE ( 'NONE', #4133, #1804 ) ;
#1651 = AXIS2_PLACEMENT_3D ( 'NONE', #7721, #7636, #6336 ) ;
#1652 = CARTESIAN_POINT ( 'NONE',  ( -1.312500000000000444, 4.908106850393701315, 3.316250000000001474 ) ) ;
#1653 = CIRCLE ( 'NONE', #4522, 4.805751768934915624 ) ;
#1654 = CARTESIAN_POINT ( 'NONE',  ( 3.362499999999998934, 1.750000000000000000, -6.725000000000002309 ) ) ;
#1655 = DIRECTION ( 'NONE',  ( -0.000000000000000000, -1.000000000000000000, -0.000000000000000000 ) ) ;
#1656 = CARTESIAN_POINT ( 'NONE',  ( 1.625000000000000222, 5.339000000000000412, -2.750000000000000444 ) ) ;
#1657 = ORIENTED_EDGE ( 'NONE', *, *, #4038, .T. ) ;
#1658 = VECTOR ( 'NONE', #902, 39.37007874015748143 ) ;
#1659 = CARTESIAN_POINT ( 'NONE',  ( -3.987046614173228587, 4.106701403462994726, 8.112636806013382440 ) ) ;
#1660 = EDGE_CURVE ( 'NONE', #5594, #7750, #5230, .T. ) ;
#1661 = FACE_OUTER_BOUND ( 'NONE', #3678, .T. ) ;
#1662 = EDGE_CURVE ( 'NONE', #1500, #3103, #2093, .T. ) ;
#1663 = CARTESIAN_POINT ( 'NONE',  ( 0.5365888410826438193, 2.415836454015215295, -2.990976592206287421 ) ) ;
#1664 = DIRECTION ( 'NONE',  ( -0.000000000000000000, 1.000000000000000000, -0.000000000000000000 ) ) ;
#1665 = AXIS2_PLACEMENT_3D ( 'NONE', #5595, #2410, #6825 ) ;
#1666 = VERTEX_POINT ( 'NONE', #7777 ) ;
#1667 = AXIS2_PLACEMENT_3D ( 'NONE', #5666, #489, #6290 ) ;
#1668 = PERSON_AND_ORGANIZATION_ROLE ( 'creator' ) ;
#1669 = CARTESIAN_POINT ( 'NONE',  ( -8.751021560936518753E-10, 1.365923996832131609E-16, 5.750408897959578548E-10 ) ) ;
#1670 = CARTESIAN_POINT ( 'NONE',  ( 0.7432847975395557860, 4.051926198797242584, 7.935140446388321500 ) ) ;
#1671 = CC_DESIGN_DATE_AND_TIME_ASSIGNMENT ( #7533, #1884, ( #6424 ) ) ;
#1672 = EDGE_LOOP ( 'NONE', ( #7779, #6478, #6427, #4554 ) ) ;
#1673 = CARTESIAN_POINT ( 'NONE',  ( 0.000000000000000000, 2.762500000000000178, 6.956250000000000711 ) ) ;
#1674 = ADVANCED_FACE ( 'NONE', ( #2052 ), #3916, .T. ) ;
#1675 = ORIENTED_EDGE ( 'NONE', *, *, #5023, .F. ) ;
#1676 = DIRECTION ( 'NONE',  ( -0.000000000000000000, 1.000000000000000000, -0.000000000000000000 ) ) ;
#1677 = ORIENTED_EDGE ( 'NONE', *, *, #5516, .F. ) ;
#1678 = DATE_TIME_ROLE ( 'classification_date' ) ;
#1679 = LINE ( 'NONE', #6613, #6208 ) ;
#1680 = DIRECTION ( 'NONE',  ( -0.000000000000000000, -1.000000000000000000, -0.000000000000000000 ) ) ;
#1681 = PERSON_AND_ORGANIZATION ( #572, #8041 ) ;
#1682 = ORIENTED_EDGE ( 'NONE', *, *, #4549, .T. ) ;
#1683 = EDGE_CURVE ( 'NONE', #1007, #4311, #202, .T. ) ;
#1684 = APPLICATION_CONTEXT ( 'configuration controlled 3d designs of mechanical parts and assemblies' ) ;
#1685 = CARTESIAN_POINT ( 'NONE',  ( 2.750000000000000444, 7.964000000000001300, 4.323750000000001315 ) ) ;
#1686 = CARTESIAN_POINT ( 'NONE',  ( -0.8148948558711907042, 4.979111548578501356, -5.108750000000004121 ) ) ;
#1687 = CARTESIAN_POINT ( 'NONE',  ( -0.6863513793485910286, 4.252392623524238857, 8.312718817107960234 ) ) ;
#1688 =( NAMED_UNIT ( * ) SI_UNIT ( $, .STERADIAN. ) SOLID_ANGLE_UNIT ( ) );
#1689 = CARTESIAN_POINT ( 'NONE',  ( 2.750000000000000444, 8.574153540863029832, 4.323750000000001315 ) ) ;
#1690 = DATE_AND_TIME ( #7324, #5900 ) ;
#1691 = ORIENTED_EDGE ( 'NONE', *, *, #3137, .T. ) ;
#1692 = CARTESIAN_POINT ( 'NONE',  ( 3.762484563843161212, 1.281112611882646579, -9.215429355903707278E-16 ) ) ;
#1693 = CARTESIAN_POINT ( 'NONE',  ( 2.875000000000000888, 1.000000000000000222, -2.975000000000000977 ) ) ;
#1694 = EDGE_CURVE ( 'NONE', #8024, #6387, #7652, .T. ) ;
#1695 = FACE_OUTER_BOUND ( 'NONE', #439, .T. ) ;
#1696 = CARTESIAN_POINT ( 'NONE',  ( 0.000000000000000000, 3.950000000000000178, 3.691250000234376660 ) ) ;
#1697 = DIRECTION ( 'NONE',  ( 1.000000000000000000, 0.000000000000000000, -1.986798540846736797E-16 ) ) ;
#1698 = CARTESIAN_POINT ( 'NONE',  ( 1.625000000000000222, 2.499999999434268982, 2.521780125537467665 ) ) ;
#1699 = VERTEX_POINT ( 'NONE', #3401 ) ;
#1700 = DIRECTION ( 'NONE',  ( 0.08785522361217638909, -0.000000000000000000, -0.9961332539796342589 ) ) ;
#1701 = VERTEX_POINT ( 'NONE', #7134 ) ;
#1702 = LINE ( 'NONE', #1582, #6331 ) ;
#1703 = CARTESIAN_POINT ( 'NONE',  ( 1.500000000000000444, 5.414000000000000590, 0.1249999999999999029 ) ) ;
#1704 = EDGE_CURVE ( 'NONE', #5031, #963, #6531, .T. ) ;
#1705 = CARTESIAN_POINT ( 'NONE',  ( 1.318571496062992399, 2.714076811023622415, -7.382249173228347949 ) ) ;
#1706 = PRODUCT_DEFINITION_SHAPE ( 'NONE', 'NONE',  #1622 ) ;
#1707 = CARTESIAN_POINT ( 'NONE',  ( 2.740000000000001545, 8.719000000000002970, 3.823750000000002647 ) ) ;
#1708 = ORIENTED_EDGE ( 'NONE', *, *, #7050, .F. ) ;
#1709 = DATE_AND_TIME ( #7299, #2539 ) ;
#1710 = LINE ( 'NONE', #2454, #5971 ) ;
#1711 = VERTEX_POINT ( 'NONE', #1400 ) ;
#1712 = CARTESIAN_POINT ( 'NONE',  ( -2.875000000000000888, 0.000000000000000000, -2.975000000000000977 ) ) ;
#1713 = ORIENTED_EDGE ( 'NONE', *, *, #1523, .F. ) ;
#1714 = CARTESIAN_POINT ( 'NONE',  ( -4.066213280839896527, 4.383999996532201848, 8.231249998505111520 ) ) ;
#1715 = CARTESIAN_POINT ( 'NONE',  ( -2.750000000000000444, 7.521783346456694552, 3.956250000000000266 ) ) ;
#1716 = ORIENTED_EDGE ( 'NONE', *, *, #1779, .F. ) ;
#1717 = APPLICATION_PROTOCOL_DEFINITION ( 'international standard', 'config_control_design', 1994, #4444 ) ;
#1718 = CC_DESIGN_DATE_AND_TIME_ASSIGNMENT ( #393, #6674, ( #1058 ) ) ;
#1719 = DIRECTION ( 'NONE',  ( 0.000000000000000000, 0.000000000000000000, 1.000000000000000000 ) ) ;
#1720 = CALENDAR_DATE ( 2026, 8, 10 ) ;
#1721 = VERTEX_POINT ( 'NONE', #6394 ) ;
#1722 = DIRECTION ( 'NONE',  ( -0.7071067811865474617, 0.000000000000000000, 0.7071067811865474617 ) ) ;
#1723 = CARTESIAN_POINT ( 'NONE',  ( 1.187500001445445985, 5.969165905511811587, 6.858307716535433585 ) ) ;
#1724 = CARTESIAN_POINT ( 'NONE',  ( -0.6892550738286248313, 4.245699673162182108, 8.129643686836866223 ) ) ;
#1725 = DIRECTION ( 'NONE',  ( 0.000000000000000000, 0.000000000000000000, 1.000000000000000000 ) ) ;
#1726 = PERSON_AND_ORGANIZATION_ROLE ( 'classification_officer' ) ;
#1727 = ORIENTED_EDGE ( 'NONE', *, *, #5433, .T. ) ;
#1728 = DIRECTION ( 'NONE',  ( 0.000000000000000000, 0.000000000000000000, -1.000000000000000000 ) ) ;
#1729 = ADVANCED_FACE ( 'NONE', ( #4546 ), #780, .T. ) ;
#1730 =( BOUNDED_SURFACE ( )  B_SPLINE_SURFACE ( 2, 1, ( 
 ( #2708, #108 ),
 ( #4420, #7011 ),
 ( #5734, #6926 ),
 ( #3839, #4545 ),
 ( #1440, #1349 ),
 ( #3915, #6436 ),
 ( #7615, #7091 ),
 ( #2623, #5644 ),
 ( #3951, #814 ),
 ( #3313, #5816 ),
 ( #201, #1399 ) ),
 .UNSPECIFIED., .F., .F., .F. ) 
 B_SPLINE_SURFACE_WITH_KNOTS ( ( 3, 2, 2, 2, 2, 3 ),
 ( 2, 2 ),
 ( 1.337827206813319902, 1.570796326794899889, 3.141592653589790007, 4.712388980384690562, 5.497197239955629477, 5.538790940287052322 ),
 ( 0.000000000000000000, 1.000000000000000000 ),
 .UNSPECIFIED. ) 
 GEOMETRIC_REPRESENTATION_ITEM ( )  RATIONAL_B_SPLINE_SURFACE ( (
 ( 0.9260057553135141450, 0.9260057553135141450),
 ( 0.9565602018087399072, 0.9565602018087399072),
 ( 1.000000000000000000, 1.000000000000000000),
 ( 0.7071067811865479058, 0.7071067811865479058),
 ( 1.000000000000000000, 1.000000000000000000),
 ( 0.7071067811865479058, 0.7071067811865479058),
 ( 1.000000000000000000, 1.000000000000000000),
 ( 0.8536633850130399548, 0.8536633850130399548),
 ( 0.8535534732088591037, 0.8535534732088591037),
 ( 0.8535534732088591037, 0.8535534732088591037),
 ( 0.8535534732088591037, 0.8535534732088591037) ) ) 
 REPRESENTATION_ITEM ( '' )  SURFACE ( )  );
#1731 = CARTESIAN_POINT ( 'NONE',  ( 2.750000000000000888, 8.719000000000001194, 3.823750000000002647 ) ) ;
#1732 = CARTESIAN_POINT ( 'NONE',  ( 0.6000000000000015321, 3.950000000000000178, 8.981250000000001066 ) ) ;
#1733 = EDGE_CURVE ( 'NONE', #4311, #1456, #7740, .T. ) ;
#1734 = ORIENTED_EDGE ( 'NONE', *, *, #3380, .F. ) ;
#1735 = DIRECTION ( 'NONE',  ( -1.000000000000000000, -0.000000000000000000, -0.000000000000000000 ) ) ;
#1736 = ORIENTED_EDGE ( 'NONE', *, *, #4476, .F. ) ;
#1737 = CARTESIAN_POINT ( 'NONE',  ( -0.06606835743134251149, 2.325000000000000622, -3.080208333333334547 ) ) ;
#1738 = DIRECTION ( 'NONE',  ( 0.000000000000000000, -1.000000000000000000, 0.000000000000000000 ) ) ;
#1739 = CARTESIAN_POINT ( 'NONE',  ( -1.187500000000000222, 5.969165905511811587, 6.858307716535433585 ) ) ;
#1740 = ADVANCED_FACE ( 'NONE', ( #3684 ), #8129, .T. ) ;
#1741 = LINE ( 'NONE', #3632, #7125 ) ;
#1742 = VERTEX_POINT ( 'NONE', #2467 ) ;
#1743 = APPROVAL_ROLE ( '' ) ;
#1744 = CARTESIAN_POINT ( 'NONE',  ( 3.791570906296184873, 1.365923996832131609E-16, 0.7997593695958172821 ) ) ;
#1745 = DATE_AND_TIME ( #2888, #4452 ) ;
#1746 = CIRCLE ( 'NONE', #7396, 2.841000000000000636 ) ;
#1747 = CC_DESIGN_SECURITY_CLASSIFICATION ( #7802, ( #4741 ) ) ;
#1748 = ADVANCED_FACE ( 'NONE', ( #6146 ), #2381, .F. ) ;
#1749 = EDGE_LOOP ( 'NONE', ( #3009, #5625, #1716 ) ) ;
#1750 = CARTESIAN_POINT ( 'NONE',  ( 1.187500000000000000, 5.002317768095269734, 4.083473622031662309 ) ) ;
#1751 = AXIS2_PLACEMENT_3D ( 'NONE', #7281, #2758, #380 ) ;
#1752 = CC_DESIGN_APPROVAL ( #3812, ( #2798 ) ) ;
#1753 = CYLINDRICAL_SURFACE ( 'NONE', #4379, 3.874999999025058539 ) ;
#1754 = DIRECTION ( 'NONE',  ( -0.000000000000000000, 1.000000000000000000, -0.000000000000000000 ) ) ;
#1755 = EDGE_LOOP ( 'NONE', ( #4157, #7008, #1324, #6449 ) ) ;
#1756 = COORDINATED_UNIVERSAL_TIME_OFFSET ( 0, 0, .AHEAD. ) ;
#1757 = CARTESIAN_POINT ( 'NONE',  ( 3.987953385826771946, 3.674333370316266389, 8.231249998505111520 ) ) ;
#1758 = APPROVAL_DATE_TIME ( #7350, #7968 ) ;
#1759 = AXIS2_PLACEMENT_3D ( 'NONE', #6155, #7414, #6774 ) ;
#1760 = CARTESIAN_POINT ( 'NONE',  ( -2.875000000000000888, 1.000000000000000222, -2.975000000000000977 ) ) ;
#1761 = DIRECTION ( 'NONE',  ( 0.5773502691896152950, 0.5773502691896467143, 0.5773502691896152950 ) ) ;
#1762 = AXIS2_PLACEMENT_3D ( 'NONE', #4335, #4837, #1188 ) ;
#1763 = ORIENTED_EDGE ( 'NONE', *, *, #562, .F. ) ;
#1764 = CARTESIAN_POINT ( 'NONE',  ( -0.7314405957411594938, 4.116041651862893502, 8.496183445665876022 ) ) ;
#1765 =( NAMED_UNIT ( * ) PLANE_ANGLE_UNIT ( ) SI_UNIT ( $, .RADIAN. ) );
#1766 = CARTESIAN_POINT ( 'NONE',  ( -8.751021560936518753E-10, 1.365923996832131609E-16, 5.750408897959578548E-10 ) ) ;
#1767 = CIRCLE ( 'NONE', #6862, 1.624999999999999778 ) ;
#1768 = PERSON_AND_ORGANIZATION_ROLE ( 'design_owner' ) ;
#1769 = EDGE_LOOP ( 'NONE', ( #5268, #3911, #4916 ) ) ;
#1770 = CARTESIAN_POINT ( 'NONE',  ( -3.874999999933440797, 1.000000000000000222, -5.476399496138180442E-16 ) ) ;
#1771 = AXIS2_PLACEMENT_3D ( 'NONE', #285, #1520, #4075 ) ;
#1772 = MANIFOLD_SOLID_BREP ( 'N', #7427 ) ;
#1773 = CC_DESIGN_PERSON_AND_ORGANIZATION_ASSIGNMENT ( #4480, #6381, ( #2137 ) ) ;
#1774 = PRODUCT ( 'bench vise-', 'bench vise-', '', ( #6614 ) ) ;
#1775 = EDGE_LOOP ( 'NONE', ( #6851, #3554, #2147, #5382 ) ) ;
#1776 = LINE ( 'NONE', #5529, #7957 ) ;
#1777 = CARTESIAN_POINT ( 'NONE',  ( -0.7335700376807066103, 2.500000000063059780, 2.750000000000000888 ) ) ;
#1778 = EDGE_CURVE ( 'NONE', #520, #7817, #8172, .T. ) ;
#1779 = EDGE_CURVE ( 'NONE', #4445, #5331, #6765, .T. ) ;
#1780 = AXIS2_PLACEMENT_3D ( 'NONE', #4970, #5661, #635 ) ;
#1781 = ORIENTED_EDGE ( 'NONE', *, *, #7046, .T. ) ;
#1782 = PLANE ( 'NONE',  #4212 ) ;
#1783 = ORIENTED_EDGE ( 'NONE', *, *, #177, .T. ) ;
#1784 = ADVANCED_FACE ( 'NONE', ( #1220 ), #4949, .T. ) ;
#1785 = CARTESIAN_POINT ( 'NONE',  ( 3.987953385826772390, 4.068613208430805095, 8.074548610981311825 ) ) ;
#1786 = DIRECTION ( 'NONE',  ( 1.000000000000000000, -0.000000000000000000, 0.000000000000000000 ) ) ;
#1787 = PLANE ( 'NONE',  #6991 ) ;
#1788 = PLANE ( 'NONE',  #1780 ) ;
#1789 = ORIENTED_EDGE ( 'NONE', *, *, #2647, .F. ) ;
#1790 = APPROVAL_ROLE ( '' ) ;
#1791 = DIRECTION ( 'NONE',  ( 0.000000000000000000, -1.000000000000000000, 0.000000000000000000 ) ) ;
#1792 =( REPRESENTATION_RELATIONSHIP ('NONE','NONE', #3570, #5548 ) REPRESENTATION_RELATIONSHIP_WITH_TRANSFORMATION ( #3262 )SHAPE_REPRESENTATION_RELATIONSHIP( ) );
#1793 = VERTEX_POINT ( 'NONE', #2502 ) ;
#1794 = AXIS2_PLACEMENT_3D ( 'NONE', #431, #2925, #3636 ) ;
#1795 = CONICAL_SURFACE ( 'NONE', #1139, 3.343750000040417447, 0.4297622790966887374 ) ;
#1796 = DIRECTION ( 'NONE',  ( 1.000000000000000000, 0.000000000000000000, 0.000000000000000000 ) ) ;
#1797 = CARTESIAN_POINT ( 'NONE',  ( -4.462046614173229564, 4.146499994074616779, 7.838250042232624004 ) ) ;
#1798 = EDGE_CURVE ( 'NONE', #6749, #4596, #1269, .T. ) ;
#1799 = ORIENTED_EDGE ( 'NONE', *, *, #2882, .T. ) ;
#1800 = DATE_TIME_ROLE ( 'classification_date' ) ;
#1801 = FACE_OUTER_BOUND ( 'NONE', #7418, .T. ) ;
#1802 = APPROVAL_ROLE ( '' ) ;
#1803 = CIRCLE ( 'NONE', #3317, 0.2625000000000008438 ) ;
#1804 = VECTOR ( 'NONE', #1041, 39.37007874015748143 ) ;
#1805 = DIRECTION ( 'NONE',  ( 0.000000000000000000, 1.000000000000000000, -0.000000000000000000 ) ) ;
#1806 = DIRECTION ( 'NONE',  ( -1.000000000000000000, 0.000000000000000000, 0.000000000000000000 ) ) ;
#1807 = DIRECTION ( 'NONE',  ( 0.000000000000000000, 0.000000000000000000, 1.000000000000000000 ) ) ;
#1808 = ORIENTED_EDGE ( 'NONE', *, *, #7675, .F. ) ;
#1809 = CARTESIAN_POINT ( 'NONE',  ( 4.470366332363715500, 1.365923996832131609E-16, 2.937534001674281914 ) ) ;
#1810 = EDGE_CURVE ( 'NONE', #5001, #1117, #4252, .T. ) ;
#1811 = CARTESIAN_POINT ( 'NONE',  ( 0.000000000000000000, 5.414000000000000590, 0.5414159055118109576 ) ) ;
#1812 = CALENDAR_DATE ( 2026, 8, 10 ) ;
#1813 = EDGE_LOOP ( 'NONE', ( #4739, #6012, #6904, #1474, #6779 ) ) ;
#1814 = FACE_OUTER_BOUND ( 'NONE', #3693, .T. ) ;
#1815 = ORIENTED_EDGE ( 'NONE', *, *, #6447, .F. ) ;
#1816 = CARTESIAN_POINT ( 'NONE',  ( -2.946793808642157231, 2.500000000130568889, -0.5624999991015005030 ) ) ;
#1817 = DIRECTION ( 'NONE',  ( 0.000000000000000000, 1.000000000000000000, 0.000000000000000000 ) ) ;
#1818 = ORIENTED_EDGE ( 'NONE', *, *, #5751, .F. ) ;
#1819 = CC_DESIGN_PERSON_AND_ORGANIZATION_ASSIGNMENT ( #1567, #7103, ( #1914 ) ) ;
#1820 = ORIENTED_EDGE ( 'NONE', *, *, #3088, .T. ) ;
#1821 = EDGE_CURVE ( 'NONE', #2706, #5748, #5847, .T. ) ;
#1822 = CARTESIAN_POINT ( 'NONE',  ( 3.296097360936645959, 1.749999999910763826, -0.5625000000000002220 ) ) ;
#1823 = CARTESIAN_POINT ( 'NONE',  ( 0.03453472440944883176, 5.297609015748031780, -5.034819094488189428 ) ) ;
#1824 = CARTESIAN_POINT ( 'NONE',  ( 1.187499999999999778, 4.894190003925942278, 5.057715191908433106 ) ) ;
#1825 = ORIENTED_EDGE ( 'NONE', *, *, #2675, .T. ) ;
#1826 = PERSON_AND_ORGANIZATION ( #7862, #8117 ) ;
#1827 = DIRECTION ( 'NONE',  ( -0.000000000000000000, -0.000000000000000000, -1.000000000000000000 ) ) ;
#1828 = FACE_OUTER_BOUND ( 'NONE', #3259, .T. ) ;
#1829 = PLANE ( 'NONE',  #5952 ) ;
#1830 = CARTESIAN_POINT ( 'NONE',  ( 0.000000000000000000, 3.950000000000000178, -5.108750000000001457 ) ) ;
#1831 = EDGE_LOOP ( 'NONE', ( #7332, #315, #3326, #1083 ) ) ;
#1832 = SECURITY_CLASSIFICATION ( '', '', #3523 ) ;
#1833 = APPROVAL_ROLE ( '' ) ;
#1834 = ADVANCED_FACE ( 'NONE', ( #7491 ), #1921, .T. ) ;
#1835 = LINE ( 'NONE', #522, #5559 ) ;
#1836 = DATE_AND_TIME ( #7487, #932 ) ;
#1837 = PRODUCT_DEFINITION_SHAPE ( 'NONE', 'NONE',  #8194 ) ;
#1838 = DIRECTION ( 'NONE',  ( 1.000000000000000000, 0.000000000000000000, 0.000000000000000000 ) ) ;
#1839 = DIRECTION ( 'NONE',  ( 0.000000000000000000, -0.000000000000000000, 1.000000000000000000 ) ) ;
#1840 = VERTEX_POINT ( 'NONE', #495 ) ;
#1841 = CARTESIAN_POINT ( 'NONE',  ( -0.6817881100752513079, 4.262513956817777228, 8.241141111267666020 ) ) ;
#1842 = CARTESIAN_POINT ( 'NONE',  ( -3.296097360993826886, 1.750000000000000444, -0.5624999982030005619 ) ) ;
#1843 = PERSON_AND_ORGANIZATION_ROLE ( 'creator' ) ;
#1844 = VERTEX_POINT ( 'NONE', #4415 ) ;
#1845 = DIRECTION ( 'NONE',  ( -0.7071067811865474617, -0.7071067811865474617, 0.000000000000000000 ) ) ;
#1846 = MANIFOLD_SOLID_BREP ( 'Imported1', #2029 ) ;
#1847 = ORIENTED_EDGE ( 'NONE', *, *, #1005, .T. ) ;
#1848 = FACE_OUTER_BOUND ( 'NONE', #1936, .T. ) ;
#1849 = DIRECTION ( 'NONE',  ( -0.000000000000000000, -0.000000000000000000, 1.000000000000000000 ) ) ;
#1850 = ORIENTED_EDGE ( 'NONE', *, *, #5686, .F. ) ;
#1851 = LINE ( 'NONE', #7852, #5531 ) ;
#1852 = EDGE_LOOP ( 'NONE', ( #5633, #153, #645, #2099, #2845, #4446, #5523, #3750, #6863, #1861, #5608, #5761 ) ) ;
#1853 = CC_DESIGN_DATE_AND_TIME_ASSIGNMENT ( #247, #7778, ( #6586 ) ) ;
#1854 = CARTESIAN_POINT ( 'NONE',  ( 3.987953385826771946, 4.084155844093235288, 8.087511858761496697 ) ) ;
#1855 = DIRECTION ( 'NONE',  ( 0.000000000000000000, 0.000000000000000000, 1.000000000000000000 ) ) ;
#1856 = DIRECTION ( 'NONE',  ( 0.000000000000000000, -0.000000000000000000, 1.000000000000000000 ) ) ;
#1857 = VERTEX_POINT ( 'NONE', #6224 ) ;
#1858 = ADVANCED_FACE ( 'NONE', ( #6264 ), #4988, .F. ) ;
#1859 = APPLICATION_PROTOCOL_DEFINITION ( 'international standard', 'config_control_design', 1994, #5975 ) ;
#1860 = DIRECTION ( 'NONE',  ( -1.000000000000000000, 0.000000000000000000, 0.000000000000000000 ) ) ;
#1861 = ORIENTED_EDGE ( 'NONE', *, *, #1873, .T. ) ;
#1862 = APPROVAL ( #7041, 'UNSPECIFIED' ) ;
#1863 = CARTESIAN_POINT ( 'NONE',  ( 0.000000000000000000, 8.719000000000001194, 3.323750000000001759 ) ) ;
#1864 = FACE_OUTER_BOUND ( 'NONE', #5147, .T. ) ;
#1865 = CARTESIAN_POINT ( 'NONE',  ( 1.625000000000000222, 2.359134605886186620, 2.598586947110950174 ) ) ;
#1866 = AXIS2_PLACEMENT_3D ( 'NONE', #2543, #5030, #5687 ) ;
#1867 = ORIENTED_EDGE ( 'NONE', *, *, #6601, .F. ) ;
#1868 = APPROVAL_DATE_TIME ( #4366, #8089 ) ;
#1869 = DIRECTION ( 'NONE',  ( -0.000000000000000000, -0.000000000000000000, 1.000000000000000000 ) ) ;
#1870 = LOCAL_TIME ( 0, 37, 23.00000000000000000, #1756 ) ;
#1871 = DATE_AND_TIME ( #4985, #6333 ) ;
#1872 = CARTESIAN_POINT ( 'NONE',  ( -2.740000000000001545, 7.964000000000000412, 3.833750000000001545 ) ) ;
#1873 = EDGE_CURVE ( 'NONE', #5810, #3375, #3238, .T. ) ;
#1874 = AXIS2_PLACEMENT_3D ( 'NONE', #1344, #3835, #1807 ) ;
#1875 = AXIS2_PLACEMENT_3D ( 'NONE', #6262, #2535, #4486 ) ;
#1876 = EDGE_CURVE ( 'NONE', #2620, #6635, #5770, .T. ) ;
#1877 = PRODUCT_DEFINITION_FORMATION_WITH_SPECIFIED_SOURCE ( 'ANY', '', #5745, .NOT_KNOWN. ) ;
#1878 = CARTESIAN_POINT ( 'NONE',  ( -3.987046614173229475, 3.769737734435318899, 8.152751440555805473 ) ) ;
#1879 = CARTESIAN_POINT ( 'NONE',  ( -2.750000000000000888, 7.964000000000000412, 3.813750000000002416 ) ) ;
#1880 = ORIENTED_EDGE ( 'NONE', *, *, #6956, .T. ) ;
#1881 = CARTESIAN_POINT ( 'NONE',  ( -1.312500000000000444, 5.969165905511811587, 0.5414159055118118458 ) ) ;
#1882 = SECURITY_CLASSIFICATION ( '', '', #5253 ) ;
#1883 = CARTESIAN_POINT ( 'NONE',  ( -0.5199956508225699325, 5.160877715126506615, 6.858307716535431808 ) ) ;
#1884 = DATE_TIME_ROLE ( 'creation_date' ) ;
#1885 = EDGE_LOOP ( 'NONE', ( #5087, #6100, #4600, #6602 ) ) ;
#1886 = VECTOR ( 'NONE', #2351, 39.37007874015748854 ) ;
#1887 = DIRECTION ( 'NONE',  ( 0.000000000000000000, -1.000000000000000000, 0.000000000000000000 ) ) ;
#1888 = AXIS2_PLACEMENT_3D ( 'NONE', #4083, #6619, #331 ) ;
#1889 = AXIS2_PLACEMENT_3D ( 'NONE', #6156, #2308, #7416 ) ;
#1890 = DIRECTION ( 'NONE',  ( 0.000000000000000000, 0.000000000000000000, -1.000000000000000000 ) ) ;
#1891 = EDGE_CURVE ( 'NONE', #6458, #1952, #772, .T. ) ;
#1892 = ORIENTED_EDGE ( 'NONE', *, *, #2792, .T. ) ;
#1893 = VECTOR ( 'NONE', #5936, 39.37007874015748143 ) ;
#1894 = ORIENTED_EDGE ( 'NONE', *, *, #1105, .T. ) ;
#1895 = AXIS2_PLACEMENT_3D ( 'NONE', #5796, #5918, #5295 ) ;
#1896 = CARTESIAN_POINT ( 'NONE',  ( 3.987953385826772390, 4.133008534184493321, 8.159690390570387919 ) ) ;
#1897 = CLOSED_SHELL ( 'NONE', ( #3279, #836, #5843, #5088 ) ) ;
#1898 = DIRECTION ( 'NONE',  ( 0.7071067811865474617, -0.7071067811865474617, -0.000000000000000000 ) ) ;
#1899 = LOCAL_TIME ( 0, 37, 23.00000000000000000, #3601 ) ;
#1900 = CARTESIAN_POINT ( 'NONE',  ( 1.187500000000000444, 4.399518635675126355, 6.597653535770707123 ) ) ;
#1901 = VERTEX_POINT ( 'NONE', #5685 ) ;
#1902 = DATE_TIME_ROLE ( 'creation_date' ) ;
#1903 = DIRECTION ( 'NONE',  ( 0.000000000000000000, -1.000000000000000000, 0.000000000000000000 ) ) ;
#1904 = EDGE_LOOP ( 'NONE', ( #5706, #4163 ) ) ;
#1905 = VECTOR ( 'NONE', #4067, 39.37007874015748143 ) ;
#1906 = CARTESIAN_POINT ( 'NONE',  ( 2.740000000000001545, 8.729000000000002757, 3.833750000000001545 ) ) ;
#1907 = CARTESIAN_POINT ( 'NONE',  ( -2.749999999999998668, 8.589000000000000412, 2.411250000000000782 ) ) ;
#1908 = CARTESIAN_POINT ( 'NONE',  ( -3.562500000000000444, 1.000000000000000222, 3.337500000000003020 ) ) ;
#1909 = ORIENTED_EDGE ( 'NONE', *, *, #2354, .F. ) ;
#1910 = AXIS2_PLACEMENT_3D ( 'NONE', #4811, #4143, #4185 ) ;
#1911 = PERSON_AND_ORGANIZATION ( #7862, #8117 ) ;
#1912 = DIRECTION ( 'NONE',  ( 1.000000000000000000, 0.000000000000000000, 0.000000000000000000 ) ) ;
#1913 = COORDINATED_UNIVERSAL_TIME_OFFSET ( 0, 0, .AHEAD. ) ;
#1914 = PRODUCT_DEFINITION ( 'UNKNOWN', '', #449, #2909 ) ;
#1915 = DIRECTION ( 'NONE',  ( 0.000000000000000000, 0.000000000000000000, -1.000000000000000000 ) ) ;
#1916 = VECTOR ( 'NONE', #3169, 39.37007874015748143 ) ;
#1917 = VECTOR ( 'NONE', #8001, 39.37007874015748143 ) ;
#1918 = CIRCLE ( 'NONE', #611, 0.3625000012227142521 ) ;
#1919 = EDGE_CURVE ( 'NONE', #7750, #8146, #4401, .T. ) ;
#1920 = CARTESIAN_POINT ( 'NONE',  ( -3.987046614173228587, 3.783676849830932110, 8.126559114045873500 ) ) ;
#1921 = CYLINDRICAL_SURFACE ( 'NONE', #2572, 3.874999999025058095 ) ;
#1922 = DIRECTION ( 'NONE',  ( -1.000000000000000000, 0.000000000000000000, 0.000000000000000000 ) ) ;
#1923 = VERTEX_POINT ( 'NONE', #1995 ) ;
#1924 = CARTESIAN_POINT ( 'NONE',  ( -3.987046614173229031, 3.674333370316265501, 8.782583289749323896 ) ) ;
#1925 = LENGTH_MEASURE_WITH_UNIT ( LENGTH_MEASURE( 0.02539999999999999897 ), #8177 );
#1926 = CARTESIAN_POINT ( 'NONE',  ( -1.187499999443275334, 5.002317768720649482, 4.083473622047245399 ) ) ;
#1927 = CALENDAR_DATE ( 2026, 8, 10 ) ;
#1928 = ORIENTED_EDGE ( 'NONE', *, *, #4278, .F. ) ;
#1929 = PLANE ( 'NONE',  #1260 ) ;
#1930 = EDGE_CURVE ( 'NONE', #5914, #1364, #7027, .T. ) ;
#1931 = EDGE_CURVE ( 'NONE', #2515, #6380, #4914, .T. ) ;
#1932 = CARTESIAN_POINT ( 'NONE',  ( 2.750000000000000444, 8.719000000000002970, 3.833750000000001545 ) ) ;
#1933 = CARTESIAN_POINT ( 'NONE',  ( 4.462953385826772035, 4.146499994074615003, 8.231249998505111520 ) ) ;
#1934 = LINE ( 'NONE', #4426, #2153 ) ;
#1935 = DIRECTION ( 'NONE',  ( -0.000000000000000000, -0.000000000000000000, -1.000000000000000000 ) ) ;
#1936 = EDGE_LOOP ( 'NONE', ( #106, #5927, #3698, #4586 ) ) ;
#1937 = EDGE_CURVE ( 'NONE', #1923, #4674, #6366, .T. ) ;
#1938 = VERTEX_POINT ( 'NONE', #1306 ) ;
#1939 = APPROVAL_PERSON_ORGANIZATION ( #152, #1208, #3728 ) ;
#1940 =( REPRESENTATION_RELATIONSHIP ('NONE','NONE', #3256, #2780 ) REPRESENTATION_RELATIONSHIP_WITH_TRANSFORMATION ( #1463 )SHAPE_REPRESENTATION_RELATIONSHIP( ) );
#1941 = EDGE_CURVE ( 'NONE', #7519, #811, #5444, .T. ) ;
#1942 = CARTESIAN_POINT ( 'NONE',  ( 3.987953385826773278, 3.937513178173875250, 8.034748693519857099 ) ) ;
#1943 = CARTESIAN_POINT ( 'NONE',  ( 1.303938020448307977, 3.777197438547405639, -5.108750000000002345 ) ) ;
#1944 = CARTESIAN_POINT ( 'NONE',  ( 1.187499999999999334, 4.294112494781764156, 6.748660968904401258 ) ) ;
#1945 = VERTEX_POINT ( 'NONE', #2579 ) ;
#1946 = APPROVAL_DATE_TIME ( #5544, #4714 ) ;
#1947 = CARTESIAN_POINT ( 'NONE',  ( 3.987953385826772834, 3.769737734436292342, 8.309748556456428403 ) ) ;
#1948 = ORIENTED_EDGE ( 'NONE', *, *, #3536, .F. ) ;
#1949 = DIRECTION ( 'NONE',  ( 0.000000000000000000, 0.000000000000000000, -1.000000000000000000 ) ) ;
#1950 = CARTESIAN_POINT ( 'NONE',  ( 1.312500000000000444, 4.908106850393701315, 2.750000000234376074 ) ) ;
#1951 = CARTESIAN_POINT ( 'NONE',  ( 0.000000000000000000, 3.950000000000000178, 2.749999998413802604 ) ) ;
#1952 = VERTEX_POINT ( 'NONE', #104 ) ;
#1953 = CALENDAR_DATE ( 2026, 8, 10 ) ;
#1954 = CARTESIAN_POINT ( 'NONE',  ( -3.687499989627468722, 1.365923996832131609E-16, 3.874999999790587513 ) ) ;
#1955 = EDGE_CURVE ( 'NONE', #4397, #4996, #5145, .T. ) ;
#1956 = APPROVAL_ROLE ( '' ) ;
#1957 = CARTESIAN_POINT ( 'NONE',  ( 2.946793809113656959, 2.499999999120089189, 0.5624999991014997258 ) ) ;
#1958 = CYLINDRICAL_SURFACE ( 'NONE', #5993, 0.3125000000000016653 ) ;
#1959 = DIRECTION ( 'NONE',  ( -0.000000000000000000, 1.000000000000000000, -0.000000000000000000 ) ) ;
#1960 = CC_DESIGN_PERSON_AND_ORGANIZATION_ASSIGNMENT ( #4149, #4858, ( #1058 ) ) ;
#1961 = DIRECTION ( 'NONE',  ( -0.7071067811865395791, 5.050217624812654886E-16, 0.7071067811865554553 ) ) ;
#1962 = VERTEX_POINT ( 'NONE', #6389 ) ;
#1963 = CARTESIAN_POINT ( 'NONE',  ( 2.750000000000000888, 8.719000000000001194, 3.333750000000001990 ) ) ;
#1964 = CARTESIAN_POINT ( 'NONE',  ( -2.750000000000000444, 7.531471846334603981, 3.702890677416158294 ) ) ;
#1965 = VERTEX_POINT ( 'NONE', #3270 ) ;
#1966 = CARTESIAN_POINT ( 'NONE',  ( -1.187500000000000666, 4.894061234189001297, 5.058487564149448446 ) ) ;
#1967 = PERSON_AND_ORGANIZATION ( #7862, #8117 ) ;
#1968 = ORIENTED_EDGE ( 'NONE', *, *, #8016, .F. ) ;
#1969 = CARTESIAN_POINT ( 'NONE',  ( 0.000000000000000000, 1.750000000000000444, 2.693920355039552791E-42 ) ) ;
#1970 = EDGE_CURVE ( 'NONE', #2664, #7024, #6430, .T. ) ;
#1971 = CC_DESIGN_PERSON_AND_ORGANIZATION_ASSIGNMENT ( #4198, #4119, ( #2360 ) ) ;
#1972 = CARTESIAN_POINT ( 'NONE',  ( 2.537500000000000533, 2.500000000000000444, 0.000000000000000000 ) ) ;
#1973 = APPROVAL_PERSON_ORGANIZATION ( #3690, #4313, #4956 ) ;
#1974 = DIRECTION ( 'NONE',  ( 0.000000000000000000, 0.000000000000000000, -1.000000000000000000 ) ) ;
#1975 = DIRECTION ( 'NONE',  ( 1.000000000000000000, 0.000000000000000000, 0.000000000000000000 ) ) ;
#1976 = ORIENTED_EDGE ( 'NONE', *, *, #1660, .T. ) ;
#1977 = EDGE_CURVE ( 'NONE', #1952, #266, #867, .T. ) ;
#1978 = ORIENTED_EDGE ( 'NONE', *, *, #113, .T. ) ;
#1979 = ADVANCED_FACE ( 'NONE', ( #934 ), #6566, .F. ) ;
#1980 = EDGE_CURVE ( 'NONE', #1286, #8146, #7211, .T. ) ;
#1981 = CARTESIAN_POINT ( 'NONE',  ( 3.987953385826772390, 3.999111350882339266, 8.039351542753342628 ) ) ;
#1982 = CARTESIAN_POINT ( 'NONE',  ( 0.4616491041369191750, 2.720615487789157072, -5.108750000000005009 ) ) ;
#1983 = CARTESIAN_POINT ( 'NONE',  ( 1.124999999999999556, 3.950000000000000178, 6.956250000000000711 ) ) ;
#1984 = CARTESIAN_POINT ( 'NONE',  ( -1.312500000205861328, 4.908106857015235747, -5.108750000000001457 ) ) ;
#1985 = ORIENTED_EDGE ( 'NONE', *, *, #7148, .T. ) ;
#1986 = DIRECTION ( 'NONE',  ( 0.000000000000000000, -0.000000000000000000, 1.000000000000000000 ) ) ;
#1987 = FACE_OUTER_BOUND ( 'NONE', #2336, .T. ) ;
#1988 = EDGE_LOOP ( 'NONE', ( #6196, #2281, #7287, #1542 ) ) ;
#1989 = APPLICATION_PROTOCOL_DEFINITION ( 'international standard', 'config_control_design', 1994, #1108 ) ;
#1990 = DIRECTION ( 'NONE',  ( 0.000000000000000000, 0.000000000000000000, -1.000000000000000000 ) ) ;
#1991 = DATE_TIME_ROLE ( 'classification_date' ) ;
#1992 = CARTESIAN_POINT ( 'NONE',  ( 2.724999998660272205, 3.550000000000001155, -1.169467086614173645 ) ) ;
#1993 = VERTEX_POINT ( 'NONE', #6013 ) ;
#1994 = CARTESIAN_POINT ( 'NONE',  ( 2.724999998660272205, 3.550000000000001155, 0.3883559095726499266 ) ) ;
#1995 = CARTESIAN_POINT ( 'NONE',  ( -1.249999999999999556, 3.950000000000000178, -4.308749999765625560 ) ) ;
#1996 = LOCAL_TIME ( 0, 37, 23.00000000000000000, #5216 ) ;
#1997 = CARTESIAN_POINT ( 'NONE',  ( 2.537499998660271761, 3.550000000000001155, 0.3883559095726499266 ) ) ;
#1998 = VERTEX_POINT ( 'NONE', #3477 ) ;
#1999 = FACE_OUTER_BOUND ( 'NONE', #851, .T. ) ;
#2000 = CARTESIAN_POINT ( 'NONE',  ( -1.187500000000000666, 4.275203145064813803, 6.771338133077573929 ) ) ;
#2001 = CARTESIAN_POINT ( 'NONE',  ( -1.124999999999999556, 3.950000000000000178, 6.956250000000000711 ) ) ;
#2002 = COORDINATED_UNIVERSAL_TIME_OFFSET ( 0, 0, .AHEAD. ) ;
#2003 = CARTESIAN_POINT ( 'NONE',  ( 2.750000000000003109, 7.339000000000003077, 2.411250000000000782 ) ) ;
#2004 = ORIENTED_EDGE ( 'NONE', *, *, #5623, .F. ) ;
#2005 = DIRECTION ( 'NONE',  ( -1.000000000000000000, -0.000000000000000000, -0.000000000000000000 ) ) ;
#2006 = CIRCLE ( 'NONE', #6604, 0.4312500000000004663 ) ;
#2007 = CC_DESIGN_SECURITY_CLASSIFICATION ( #6195, ( #303 ) ) ;
#2008 = CARTESIAN_POINT ( 'NONE',  ( 1.625000000000000222, 2.500000000000000000, 2.750000000000000444 ) ) ;
#2009 = AXIS2_PLACEMENT_3D ( 'NONE', #5325, #7232, #1613 ) ;
#2010 = LENGTH_MEASURE_WITH_UNIT ( LENGTH_MEASURE( 0.02539999999999999897 ), #7657 );
#2011 = CARTESIAN_POINT ( 'NONE',  ( -2.745000000000000551, 8.724000000000001975, 3.333750000000001990 ) ) ;
#2012 = ORIENTED_EDGE ( 'NONE', *, *, #3139, .T. ) ;
#2013 = CARTESIAN_POINT ( 'NONE',  ( 2.750000000000000888, 8.729000000000002757, 3.813750000000002416 ) ) ;
#2014 = ORIENTED_EDGE ( 'NONE', *, *, #3180, .F. ) ;
#2015 = CC_DESIGN_PERSON_AND_ORGANIZATION_ASSIGNMENT ( #5592, #1205, ( #3896 ) ) ;
#2016 = CIRCLE ( 'NONE', #839, 0.2625000000000008438 ) ;
#2017 =( GEOMETRIC_REPRESENTATION_CONTEXT ( 3 ) GLOBAL_UNCERTAINTY_ASSIGNED_CONTEXT ( ( #5786 ) ) GLOBAL_UNIT_ASSIGNED_CONTEXT ( ( #7061, #291, #2181 ) ) REPRESENTATION_CONTEXT ( 'NONE', 'WORKASPACE' ) );
#2018 = ADVANCED_FACE ( 'N', ( #3999 ), #397, .T. ) ;
#2019 = CARTESIAN_POINT ( 'NONE',  ( 3.987953385826772834, 3.845309131479383247, 8.064926832397505407 ) ) ;
#2020 = CARTESIAN_POINT ( 'NONE',  ( 0.1740164558986418974, 5.251634619451294839, -5.108750000000001457 ) ) ;
#2021 = AXIS2_PLACEMENT_3D ( 'NONE', #5827, #4506, #5201 ) ;
#2022 = VECTOR ( 'NONE', #1546, 39.37007874015748143 ) ;
#2023 = CARTESIAN_POINT ( 'NONE',  ( 3.987953385826772834, 3.823364637257239185, 8.381772284350258673 ) ) ;
#2024 = CARTESIAN_POINT ( 'NONE',  ( 1.557862129563219122, 2.150738730688390721, 2.749999999536767437 ) ) ;
#2025 = ORIENTED_EDGE ( 'NONE', *, *, #5083, .F. ) ;
#2026 = ADVANCED_FACE ( 'NONE', ( #895 ), #7306, .T. ) ;
#2027 = AXIS2_PLACEMENT_3D ( 'NONE', #4206, #2471, #6841 ) ;
#2028 = B_SPLINE_CURVE_WITH_KNOTS ( 'NONE', 3,
 ( #5463, #4854, #7379, #6748 ),
 .UNSPECIFIED., .F., .F.,
 ( 4, 4 ),
 ( 0.000000000000000000, 0.01222568466273604368 ),
 .UNSPECIFIED. ) ;
#2029 = CLOSED_SHELL ( 'NONE', ( #1536, #515, #2695, #4882 ) ) ;
#2030 = FACE_BOUND ( 'NONE', #3861, .T. ) ;
#2031 = LINE ( 'NONE', #3, #5682 ) ;
#2032 = ORIENTED_EDGE ( 'NONE', *, *, #8040, .F. ) ;
#2033 = APPLICATION_PROTOCOL_DEFINITION ( 'international standard', 'config_control_design', 1994, #3147 ) ;
#2034 = DIRECTION ( 'NONE',  ( -0.000000000000000000, -0.000000000000000000, 1.000000000000000000 ) ) ;
#2035 = APPROVAL_ROLE ( '' ) ;
#2036 = CARTESIAN_POINT ( 'NONE',  ( 0.7371834602650289003, 3.810622082980045455, 7.950806627216492117 ) ) ;
#2037 = CIRCLE ( 'NONE', #1525, 1.624999999999999778 ) ;
#2038 = CARTESIAN_POINT ( 'NONE',  ( 0.7335374419612978869, 4.107240241069344044, 8.502074107329821828 ) ) ;
#2039 = CARTESIAN_POINT ( 'NONE',  ( -8.751021560936518753E-10, 1.365923996832131609E-16, 5.750408897959578548E-10 ) ) ;
#2040 =( BOUNDED_CURVE ( )  B_SPLINE_CURVE ( 3, ( #6337, #2650, #5133, #52 ),
 .UNSPECIFIED., .F., .F. ) 
 B_SPLINE_CURVE_WITH_KNOTS ( ( 4, 4 ),
 ( 0.000000000000000000, 1.000000000000000000 ),
 .UNSPECIFIED. ) 
 CURVE ( )  GEOMETRIC_REPRESENTATION_ITEM ( )  RATIONAL_B_SPLINE_CURVE ( ( 1.000000000000000000, 0.3333333333333334259, 0.3333333333333334259, 1.000000000000000000 ) ) 
 REPRESENTATION_ITEM ( '' )  );
#2041 = EDGE_LOOP ( 'NONE', ( #4332, #1397, #7612, #6170, #4087, #7748, #2793, #6161 ) ) ;
#2042 = ADVANCED_FACE ( 'NONE', ( #6603 ), #5754, .T. ) ;
#2043 = CARTESIAN_POINT ( 'NONE',  ( -3.987046614173230363, 3.766726267967030140, 8.160372747217270017 ) ) ;
#2044 = EDGE_CURVE ( 'NONE', #615, #1469, #1021, .T. ) ;
#2045 = CARTESIAN_POINT ( 'NONE',  ( 1.312500000000000444, 5.969165905511811587, 3.161250000000001670 ) ) ;
#2046 = CARTESIAN_POINT ( 'NONE',  ( -3.987046614173229475, 4.126152250297099755, 8.318774035909180853 ) ) ;
#2047 = ORIENTED_EDGE ( 'NONE', *, *, #5849, .F. ) ;
#2048 = LINE ( 'NONE', #5689, #2419 ) ;
#2049 = ORIENTED_EDGE ( 'NONE', *, *, #3536, .T. ) ;
#2050 = CARTESIAN_POINT ( 'NONE',  ( 1.407055448668504072, 2.812660052342380368, 8.674522324930370232 ) ) ;
#2051 = DIRECTION ( 'NONE',  ( 0.000000000000000000, -0.000000000000000000, 1.000000000000000000 ) ) ;
#2052 = FACE_OUTER_BOUND ( 'NONE', #991, .T. ) ;
#2053 = APPROVAL_STATUS ( 'not_yet_approved' ) ;
#2054 = EDGE_LOOP ( 'NONE', ( #2935, #5695 ) ) ;
#2055 = AXIS2_PLACEMENT_3D ( 'NONE', #1598, #4034, #2891 ) ;
#2056 = AXIS2_PLACEMENT_3D ( 'NONE', #3481, #4862, #7309 ) ;
#2057 = ADVANCED_FACE ( 'NONE', ( #2934 ), #1795, .T. ) ;
#2058 = DIRECTION ( 'NONE',  ( 0.000000000000000000, 0.000000000000000000, 1.000000000000000000 ) ) ;
#2059 = CARTESIAN_POINT ( 'NONE',  ( -2.750000000000000444, 8.589000000000000412, 3.161250000000001670 ) ) ;
#2060 = VECTOR ( 'NONE', #5021, 39.37007874015748854 ) ;
#2061 = SHAPE_REPRESENTATION_RELATIONSHIP ( 'NONE' , 'NONE' ,  #7355, #7953 ) ;
#2062 = DIRECTION ( 'NONE',  ( 1.000000000000000000, 0.000000000000000000, 0.000000000000000000 ) ) ;
#2063 = ORIENTED_EDGE ( 'NONE', *, *, #5301, .F. ) ;
#2064 = VERTEX_POINT ( 'NONE', #2208 ) ;
#2065 = DIRECTION ( 'NONE',  ( 1.000000000000000000, 0.000000000000000000, 0.000000000000000000 ) ) ;
#2066 = APPROVAL ( #2079, 'UNKNOWN' ) ;
#2067 = CARTESIAN_POINT ( 'NONE',  ( 0.5808953724622998305, 2.769908242203201976, -5.108750000000004121 ) ) ;
#2068 = DIRECTION ( 'NONE',  ( -0.7071067811865474617, 0.000000000000000000, 0.7071067811865474617 ) ) ;
#2069 = ORIENTED_EDGE ( 'NONE', *, *, #2396, .T. ) ;
#2070 = CARTESIAN_POINT ( 'NONE',  ( 3.987953385826772834, 4.128161578176055002, 8.314258565286806402 ) ) ;
#2071 = ORIENTED_EDGE ( 'NONE', *, *, #476, .T. ) ;
#2072 = LINE ( 'NONE', #1457, #6719 ) ;
#2073 = CC_DESIGN_APPROVAL ( #2908, ( #3381 ) ) ;
#2074 = CARTESIAN_POINT ( 'NONE',  ( 4.462953385826772035, 4.146499994074615003, 8.231249998505111520 ) ) ;
#2075 = LINE ( 'NONE', #6557, #3725 ) ;
#2076 = ORIENTED_EDGE ( 'NONE', *, *, #5957, .F. ) ;
#2077 = COORDINATED_UNIVERSAL_TIME_OFFSET ( 0, 0, .AHEAD. ) ;
#2078 = PLANE ( 'NONE',  #4912 ) ;
#2079 = APPROVAL_STATUS ( 'not_yet_approved' ) ;
#2080 = CARTESIAN_POINT ( 'NONE',  ( 0.6907419235105255462, 3.657778167482562903, 8.120048698298123924 ) ) ;
#2081 = CARTESIAN_POINT ( 'NONE',  ( 3.987953385826771946, 3.674333370316266389, 8.231249998505111520 ) ) ;
#2082 = ADVANCED_FACE ( 'NONE', ( #4654 ), #7170, .F. ) ;
#2083 = APPROVAL_PERSON_ORGANIZATION ( #364, #2908, #5153 ) ;
#2084 = EDGE_CURVE ( 'NONE', #586, #5647, #5715, .T. ) ;
#2085 = ORIENTED_EDGE ( 'NONE', *, *, #7938, .F. ) ;
#2086 = EDGE_CURVE ( 'NONE', #6380, #5098, #6612, .T. ) ;
#2087 = CARTESIAN_POINT ( 'NONE',  ( -3.987046614173229475, 4.084155844094571997, 8.374988138248092184 ) ) ;
#2088 = ORIENTED_EDGE ( 'NONE', *, *, #4953, .T. ) ;
#2089 = CARTESIAN_POINT ( 'NONE',  ( -3.987046614173228587, 3.950000015938371689, 8.231249998505111520 ) ) ;
#2090 = ORIENTED_EDGE ( 'NONE', *, *, #7157, .T. ) ;
#2091 = CARTESIAN_POINT ( 'NONE',  ( 0.000000000000000000, 0.000000000000000000, 0.000000000000000000 ) ) ;
#2092 = CARTESIAN_POINT ( 'NONE',  ( 0.7499999999999993339, 3.950000000000000178, 8.831250000000000711 ) ) ;
#2093 = LINE ( 'NONE', #2001, #4392 ) ;
#2094 = SECURITY_CLASSIFICATION_LEVEL ( 'unclassified' ) ;
#2095 = ORIENTED_EDGE ( 'NONE', *, *, #4977, .T. ) ;
#2096 = CARTESIAN_POINT ( 'NONE',  ( 0.000000000000000000, 5.025000000000000355, 3.742515787401575533 ) ) ;
#2097 = CARTESIAN_POINT ( 'NONE',  ( -1.500000000000000444, 5.339000000000000412, 0.1249999999999999029 ) ) ;
#2098 = CARTESIAN_POINT ( 'NONE',  ( -0.7499999999999993339, 3.950000000000000178, 8.231250000000001066 ) ) ;
#2099 = ORIENTED_EDGE ( 'NONE', *, *, #1410, .T. ) ;
#2100 = DATE_AND_TIME ( #3924, #4753 ) ;
#2101 = ORIENTED_EDGE ( 'NONE', *, *, #7167, .T. ) ;
#2102 = FACE_OUTER_BOUND ( 'NONE', #1156, .T. ) ;
#2103 = DESIGN_CONTEXT ( 'detailed design', #6968, 'design' ) ;
#2104 = ORGANIZATION ( 'NAUO-ORG11', 'UNSPECIFIED', 'UNSPECIFIED' ) ;
#2105 = CC_DESIGN_APPROVAL ( #7968, ( #1832 ) ) ;
#2106 = CARTESIAN_POINT ( 'NONE',  ( 0.000000000000000000, 3.950000000000000178, 7.231250000000000178 ) ) ;
#2107 = CARTESIAN_POINT ( 'NONE',  ( 4.462953385826773811, 4.225666661560476989, 7.679916707260901809 ) ) ;
#2108 = CARTESIAN_POINT ( 'NONE',  ( 3.987953385826773278, 4.110686350264241895, 8.344403569825947997 ) ) ;
#2109 = VERTEX_POINT ( 'NONE', #551 ) ;
#2110 = ADVANCED_FACE ( 'NONE', ( #6866 ), #6210, .T. ) ;
#2111 = CARTESIAN_POINT ( 'NONE',  ( -1.249999999999999556, 3.950000000000000178, 3.691250000234376660 ) ) ;
#2112 = VERTEX_POINT ( 'NONE', #5552 ) ;
#2113 = CALENDAR_DATE ( 2026, 8, 10 ) ;
#2114 = LINE ( 'NONE', #6516, #4251 ) ;
#2115 = DATE_AND_TIME ( #274, #5166 ) ;
#2116 = CARTESIAN_POINT ( 'NONE',  ( 3.583510604133040900, 1.543025754838327046, -8.777069582124253846E-16 ) ) ;
#2117 = CARTESIAN_POINT ( 'NONE',  ( 0.7253671533374043134, 4.140809826333097021, 8.478940687276063315 ) ) ;
#2118 = CARTESIAN_POINT ( 'NONE',  ( -2.946793808531571468, 2.500000000000000000, 0.5625000000000002220 ) ) ;
#2119 = CC_DESIGN_PERSON_AND_ORGANIZATION_ASSIGNMENT ( #3424, #1385, ( #1491 ) ) ;
#2120 = ORIENTED_EDGE ( 'NONE', *, *, #79, .F. ) ;
#2121 = CARTESIAN_POINT ( 'NONE',  ( 0.000000000000000000, 1.750000000000000666, 0.000000000000000000 ) ) ;
#2122 = CARTESIAN_POINT ( 'NONE',  ( -3.987046614173228587, 3.759071817854777287, 8.277905906474869013 ) ) ;
#2123 = ORIENTED_EDGE ( 'NONE', *, *, #5558, .F. ) ;
#2124 = DIRECTION ( 'NONE',  ( -0.000000000000000000, -1.000000000000000000, -0.000000000000000000 ) ) ;
#2125 =( NAMED_UNIT ( * ) SI_UNIT ( $, .STERADIAN. ) SOLID_ANGLE_UNIT ( ) );
#2126 = FACE_OUTER_BOUND ( 'NONE', #4568, .T. ) ;
#2127 = CALENDAR_DATE ( 2026, 8, 10 ) ;
#2128 = ORIENTED_EDGE ( 'NONE', *, *, #4762, .T. ) ;
#2129 = ADVANCED_FACE ( 'NONE', ( #6790 ), #3051, .T. ) ;
#2130 = CARTESIAN_POINT ( 'NONE',  ( -1.205291321983570585, 3.430008700001376365, -5.108749999999999680 ) ) ;
#2131 = DIRECTION ( 'NONE',  ( 0.000000000000000000, 0.000000000000000000, -1.000000000000000000 ) ) ;
#2132 = FACE_OUTER_BOUND ( 'NONE', #7370, .T. ) ;
#2133 = ORIENTED_EDGE ( 'NONE', *, *, #3380, .T. ) ;
#2134 = SECURITY_CLASSIFICATION_LEVEL ( 'unclassified' ) ;
#2135 = EDGE_LOOP ( 'NONE', ( #7466, #5348, #870, #4153 ) ) ;
#2136 = AXIS2_PLACEMENT_3D ( 'NONE', #906, #6487, #5197 ) ;
#2137 = SECURITY_CLASSIFICATION ( '', '', #799 ) ;
#2138 = CARTESIAN_POINT ( 'NONE',  ( 0.7432847975395561191, 3.848073801202759103, 8.527359553611677967 ) ) ;
#2139 =( BOUNDED_CURVE ( )  B_SPLINE_CURVE ( 3, ( #2763, #7203, #7930, #5248 ),
 .UNSPECIFIED., .F., .F. ) 
 B_SPLINE_CURVE_WITH_KNOTS ( ( 4, 4 ),
 ( 0.000000000000000000, 1.000000000000000000 ),
 .UNSPECIFIED. ) 
 CURVE ( )  GEOMETRIC_REPRESENTATION_ITEM ( )  RATIONAL_B_SPLINE_CURVE ( ( 1.000000000000000000, 0.8047378541243660477, 0.8047378541243660477, 1.000000000000000000 ) ) 
 REPRESENTATION_ITEM ( '' )  );
#2140 = ADVANCED_BREP_SHAPE_REPRESENTATION ( '', ( #7194, #7272 ), #1380 ) ;
#2141 = CIRCLE ( 'NONE', #438, 3.874999999025058539 ) ;
#2142 = PLANE ( 'NONE',  #1626 ) ;
#2143 = ADVANCED_FACE ( 'NONE', ( #8119 ), #8160, .F. ) ;
#2144 = CYLINDRICAL_SURFACE ( 'NONE', #2566, 0.1875000000000006661 ) ;
#2145 = CARTESIAN_POINT ( 'NONE',  ( 3.987953385826772390, 4.019420561376718659, 8.415080959133108607 ) ) ;
#2146 = CIRCLE ( 'NONE', #173, 1.124999999999999556 ) ;
#2147 = ORIENTED_EDGE ( 'NONE', *, *, #3549, .T. ) ;
#2148 = AXIS2_PLACEMENT_3D ( 'NONE', #7530, #147, #66 ) ;
#2149 = LOCAL_TIME ( 0, 37, 23.00000000000000000, #5947 ) ;
#2150 = CARTESIAN_POINT ( 'NONE',  ( 2.349999998660270872, 3.550000000000001155, 2.790532913385826763 ) ) ;
#2151 = AXIS2_PLACEMENT_3D ( 'NONE', #4129, #7271, #7959 ) ;
#2152 = CYLINDRICAL_SURFACE ( 'NONE', #4267, 0.7499999999999993339 ) ;
#2153 = VECTOR ( 'NONE', #2633, 39.37007874015748854 ) ;
#2154 = DIRECTION ( 'NONE',  ( -0.000000000000000000, 1.000000000000000000, -0.000000000000000000 ) ) ;
#2155 = ORIENTED_EDGE ( 'NONE', *, *, #5683, .F. ) ;
#2156 = PERSON_AND_ORGANIZATION ( #7862, #8117 ) ;
#2157 = FACE_OUTER_BOUND ( 'NONE', #5421, .T. ) ;
#2158 = CARTESIAN_POINT ( 'NONE',  ( 0.7431911064911156384, 3.848678615087431698, 7.935451190925252085 ) ) ;
#2159 = CARTESIAN_POINT ( 'NONE',  ( -8.751021560936518753E-10, 1.000000000000000222, 5.750408897959578548E-10 ) ) ;
#2160 = DIRECTION ( 'NONE',  ( 1.000000000000000000, 0.000000000000000000, 0.000000000000000000 ) ) ;
#2161 = CIRCLE ( 'NONE', #3077, 1.249999999999999556 ) ;
#2162 = CLOSED_SHELL ( 'NONE', ( #8186, #5672, #5157, #840, #2803, #4474, #4173, #1633 ) ) ;
#2163 = AXIS2_PLACEMENT_3D ( 'NONE', #4003, #2213, #5228 ) ;
#2164 = VERTEX_POINT ( 'NONE', #481 ) ;
#2165 = CARTESIAN_POINT ( 'NONE',  ( -2.375000000000000888, 2.762500000000000178, 6.956249999999999822 ) ) ;
#2166 = AXIS2_PLACEMENT_3D ( 'NONE', #56, #2575, #1990 ) ;
#2167 = CARTESIAN_POINT ( 'NONE',  ( -3.987046614173229475, 3.871501457986266104, 8.411512280006446574 ) ) ;
#2168 = DIRECTION ( 'NONE',  ( 0.000000000000000000, -0.000000000000000000, 1.000000000000000000 ) ) ;
#2169 = CARTESIAN_POINT ( 'NONE',  ( 0.000000000000000000, 2.875000000000000888, 3.440250000000001140 ) ) ;
#2170 = ORIENTED_EDGE ( 'NONE', *, *, #6517, .T. ) ;
#2171 = CC_DESIGN_DATE_AND_TIME_ASSIGNMENT ( #571, #2345, ( #1419 ) ) ;
#2172 = DIRECTION ( 'NONE',  ( 0.000000000000000000, -1.000000000000000000, 0.000000000000000000 ) ) ;
#2173 = B_SPLINE_CURVE_WITH_KNOTS ( 'NONE', 3,
 ( #1563, #3440, #5475, #2416, #2376, #7393, #4245, #3646, #4292, #5738, #2786, #4791, #1686, #6686, #5728, #2178, #329, #4010, #4667, #1564, #4590, #3958, #251, #6618, #2747, #4044, #7913, #1032, #994, #6535, #2250, #4742, #5823, #6578, #4705, #3489, #4081, #7097, #2130, #7181, #288, #2712, #944, #2828, #3442, #5943, #5902, #7222, #5318, #1605, #2785, #5273, #5990, #7782, #7138, #1478, #2868, #7874, #367, #2218, #7828 ),
 .UNSPECIFIED., .F., .F.,
 ( 4, 2, 2, 2, 2, 2, 2, 2, 2, 2, 2, 1, 2, 2, 2, 2, 2, 2, 2, 2, 2, 2, 2, 2, 2, 2, 2, 2, 2, 2, 4 ),
 ( 0.000000000000000000, 0.006512929480687936271, 0.009769394221031912212, 0.01302585896137588989, 0.01953878844206384177, 0.02116702081223586010, 0.02279525318240787496, 0.02605171792275184917, 0.03256464740343981840, 0.03419287977361179509, 0.03582111214378377179, 0.03907757688412773212, 0.04233404162447169244, 0.04396227399464366220, 0.04559050636481563890, 0.05210343584550344159, 0.05535990058584736723, 0.05698813295601932311, 0.05861636532619128592, 0.06512929480687901229, 0.06675752717705098205, 0.06838575954722293793, 0.07164222428756686356, 0.07815515376825467320, 0.08141161850859858495, 0.08466808324894249671, 0.08792454798928640847, 0.09118101272963030635, 0.09769394221031812986, 0.1009504069506620277, 0.1042068716910059117 ),
 .UNSPECIFIED. ) ;
#2174 = APPROVAL_ROLE ( '' ) ;
#2175 = ORIENTED_EDGE ( 'NONE', *, *, #5942, .T. ) ;
#2176 = AXIS2_PLACEMENT_3D ( 'NONE', #7972, #2310, #5328 ) ;
#2177 = B_SPLINE_CURVE_WITH_KNOTS ( 'NONE', 3,
 ( #5680, #5067, #4369, #1957 ),
 .UNSPECIFIED., .F., .F.,
 ( 4, 4 ),
 ( 0.000000000000000000, 0.02101476594778851903 ),
 .UNSPECIFIED. ) ;
#2178 = CARTESIAN_POINT ( 'NONE',  ( -0.9878476136873203250, 4.818414295186383534, -5.108749999999999680 ) ) ;
#2179 = CARTESIAN_POINT ( 'NONE',  ( -0.3232363751884362868, 2.357145915514489598, 3.048554855073091652 ) ) ;
#2180 = LINE ( 'NONE', #4046, #7816 ) ;
#2181 =( NAMED_UNIT ( * ) SI_UNIT ( $, .STERADIAN. ) SOLID_ANGLE_UNIT ( ) );
#2182 = LINE ( 'NONE', #415, #7550 ) ;
#2183 = VERTEX_POINT ( 'NONE', #6171 ) ;
#2184 = AXIS2_PLACEMENT_3D ( 'NONE', #3651, #8043, #7450 ) ;
#2185 = COORDINATED_UNIVERSAL_TIME_OFFSET ( 0, 0, .AHEAD. ) ;
#2186 = VERTEX_POINT ( 'NONE', #4978 ) ;
#2187 = ADVANCED_FACE ( 'N', ( #6754 ), #3640, .T. ) ;
#2188 = CIRCLE ( 'NONE', #5526, 3.874999999025058095 ) ;
#2189 = AXIS2_PLACEMENT_3D ( 'NONE', #4860, #3597, #518 ) ;
#2190 = LINE ( 'NONE', #1573, #3581 ) ;
#2191 = CARTESIAN_POINT ( 'NONE',  ( 3.987953385826771946, 3.753500037802127931, 7.838250042232624892 ) ) ;
#2192 = EDGE_CURVE ( 'NONE', #5123, #3668, #1140, .T. ) ;
#2193 = CARTESIAN_POINT ( 'NONE',  ( 3.987953385826772390, 4.068870000980494339, 8.388305332349000665 ) ) ;
#2194 = CIRCLE ( 'NONE', #753, 3.874999999025058539 ) ;
#2195 = ORIENTED_EDGE ( 'NONE', *, *, #1597, .T. ) ;
#2196 = CIRCLE ( 'NONE', #1667, 3.000000000000000888 ) ;
#2197 = CARTESIAN_POINT ( 'NONE',  ( -3.987046614173229475, 4.142924502496678762, 8.193927407620929415 ) ) ;
#2198 = FACE_OUTER_BOUND ( 'NONE', #6529, .T. ) ;
#2199 = CARTESIAN_POINT ( 'NONE',  ( -3.987046614173228587, 4.146499994074616779, 8.231249998505111520 ) ) ;
#2200 = DIRECTION ( 'NONE',  ( 0.000000000000000000, 0.000000000000000000, 1.000000000000000000 ) ) ;
#2201 = SHAPE_DEFINITION_REPRESENTATION ( #5489, #6040 ) ;
#2202 = PLANE ( 'NONE',  #852 ) ;
#2203 = DATE_AND_TIME ( #7859, #7502 ) ;
#2204 = DIRECTION ( 'NONE',  ( 1.000000000000000000, 0.000000000000000000, 0.000000000000000000 ) ) ;
#2205 = EDGE_CURVE ( 'NONE', #2109, #1857, #1406, .T. ) ;
#2206 = PRODUCT_DEFINITION_FORMATION_WITH_SPECIFIED_SOURCE ( 'ANY', '', #1182, .NOT_KNOWN. ) ;
#2207 = VERTEX_POINT ( 'NONE', #7516 ) ;
#2208 = CARTESIAN_POINT ( 'NONE',  ( -1.249999999999999556, 3.950000000000000178, 3.691250000234376660 ) ) ;
#2209 = VERTEX_POINT ( 'NONE', #8070 ) ;
#2210 = CARTESIAN_POINT ( 'NONE',  ( -2.150000000000000799, 5.025000000000000355, 3.742515787401574645 ) ) ;
#2211 = PLANE ( 'NONE',  #5579 ) ;
#2212 = EDGE_LOOP ( 'NONE', ( #2347, #1640, #5202, #2088 ) ) ;
#2213 = DIRECTION ( 'NONE',  ( 0.02399855138128190180, -0.02196770450484158282, 0.9994706046154574475 ) ) ;
#2214 = PLANE ( 'NONE',  #48 ) ;
#2215 = PERSON_AND_ORGANIZATION ( #7862, #8117 ) ;
#2216 = VERTEX_POINT ( 'NONE', #4287 ) ;
#2217 = APPROVAL ( #3183, 'UNKNOWN' ) ;
#2218 = CARTESIAN_POINT ( 'NONE',  ( -0.04453717661363842256, 2.637539714682124892, -5.108750000000001457 ) ) ;
#2219 = CARTESIAN_POINT ( 'NONE',  ( 0.1625041179141621384, 2.332820669151155712, 3.072499754721300214 ) ) ;
#2220 = DIRECTION ( 'NONE',  ( -0.000000000000000000, -0.000000000000000000, -1.000000000000000000 ) ) ;
#2221 = CARTESIAN_POINT ( 'NONE',  ( 3.875000000000001776, 1.000000000000000222, 0.000000000000000000 ) ) ;
#2222 = PERSON_AND_ORGANIZATION_ROLE ( 'creator' ) ;
#2223 = VERTEX_POINT ( 'NONE', #2370 ) ;
#2224 = APPROVAL ( #360, 'UNSPECIFIED' ) ;
#2225 = PLANE ( 'NONE',  #1493 ) ;
#2226 = DIRECTION ( 'NONE',  ( -0.000000000000000000, -0.000000000000000000, -1.000000000000000000 ) ) ;
#2227 = CARTESIAN_POINT ( 'NONE',  ( 3.121988307086614345, 2.389005866141732604, 4.968462007874016706 ) ) ;
#2228 = LINE ( 'NONE', #4095, #7395 ) ;
#2229 = VERTEX_POINT ( 'NONE', #5508 ) ;
#2230 = APPROVAL_PERSON_ORGANIZATION ( #1066, #8075, #6143 ) ;
#2231 = ADVANCED_FACE ( 'NONE', ( #1828 ), #3675, .T. ) ;
#2232 = CARTESIAN_POINT ( 'NONE',  ( 2.740000000000000657, 8.729000000000002757, 3.823750000000002647 ) ) ;
#2233 = CARTESIAN_POINT ( 'NONE',  ( -2.750000000000000444, 7.964000000000001300, 3.956249999995860911 ) ) ;
#2234 = CARTESIAN_POINT ( 'NONE',  ( -2.750000000000000444, 8.729000000000002757, 3.333750000000001990 ) ) ;
#2235 = PLANE ( 'NONE',  #7016 ) ;
#2236 = EDGE_LOOP ( 'NONE', ( #4527, #6847, #4036, #622 ) ) ;
#2237 = DATE_AND_TIME ( #430, #6606 ) ;
#2238 = CARTESIAN_POINT ( 'NONE',  ( -2.740000000000001545, 8.729000000000002757, 3.823750000000002647 ) ) ;
#2239 = CARTESIAN_POINT ( 'NONE',  ( 0.7052155605301347885, 5.414000000000000590, 0.5414159055118110686 ) ) ;
#2240 = ORIENTED_EDGE ( 'NONE', *, *, #6413, .F. ) ;
#2241 = CARTESIAN_POINT ( 'NONE',  ( -3.121988307086614345, 5.510994133858267752, 4.968462007874016706 ) ) ;
#2242 = EDGE_LOOP ( 'NONE', ( #3589, #2076 ) ) ;
#2243 = CARTESIAN_POINT ( 'NONE',  ( -3.182000000000000828, 5.541000000000003922, 3.956250000000000266 ) ) ;
#2244 = EDGE_LOOP ( 'NONE', ( #6043, #5590, #111, #1261, #4964, #3550, #2524, #270, #6251 ) ) ;
#2245 = PERSON_AND_ORGANIZATION ( #7862, #8117 ) ;
#2246 = DIRECTION ( 'NONE',  ( -0.000000000000000000, 1.000000000000000000, 0.000000000000000000 ) ) ;
#2247 = ITEM_DEFINED_TRANSFORMATION ( 'NONE', 'NONE', #2163,  #7272 ) ;
#2248 = ORIENTED_EDGE ( 'NONE', *, *, #2807, .F. ) ;
#2249 = DIRECTION ( 'NONE',  ( -1.000000000000000000, 0.000000000000000000, -0.000000000000000000 ) ) ;
#2250 = CARTESIAN_POINT ( 'NONE',  ( -1.312565957648427428, 3.909279572067391850, -5.108750000000001457 ) ) ;
#2251 = CARTESIAN_POINT ( 'NONE',  ( -0.6796865136544424368, 2.472739766459443267, 2.935403920510917253 ) ) ;
#2252 = LINE ( 'NONE', #1646, #4232 ) ;
#2253 = CARTESIAN_POINT ( 'NONE',  ( -1.312500000000001110, 7.339000000000003077, 3.239595687665816737 ) ) ;
#2254 = APPROVAL_DATE_TIME ( #5203, #6874 ) ;
#2255 = ORIENTED_EDGE ( 'NONE', *, *, #7536, .T. ) ;
#2256 = CARTESIAN_POINT ( 'NONE',  ( -2.740000000000000657, 7.969000000000000306, 3.818750000000002753 ) ) ;
#2257 = DESIGN_CONTEXT ( 'detailed design', #8182, 'design' ) ;
#2258 = DIRECTION ( 'NONE',  ( 0.000000000000000000, -1.000000000000000000, -0.000000000000000000 ) ) ;
#2259 = VECTOR ( 'NONE', #506, 39.37007874015748143 ) ;
#2260 = DIRECTION ( 'NONE',  ( 0.000000000000000000, 0.000000000000000000, 1.000000000000000000 ) ) ;
#2261 = PRODUCT_RELATED_PRODUCT_CATEGORY ( 'detail', '', ( #5745 ) ) ;
#2262 = LINE ( 'NONE', #1161, #4085 ) ;
#2263 = ORIENTED_EDGE ( 'NONE', *, *, #4730, .T. ) ;
#2264 = AXIS2_PLACEMENT_3D ( 'NONE', #178, #7719, #1503 ) ;
#2265 = CC_DESIGN_APPROVAL ( #7131, ( #5941 ) ) ;
#2266 = CARTESIAN_POINT ( 'NONE',  ( -3.987046614173228587, 4.100522301784816470, 8.104614619825735389 ) ) ;
#2267 = DIRECTION ( 'NONE',  ( -0.000000000000000000, -1.000000000000000000, 0.000000000000000000 ) ) ;
#2268 = CARTESIAN_POINT ( 'NONE',  ( 0.000000000000000000, 2.325000000000000622, -3.080208333333334103 ) ) ;
#2269 = CARTESIAN_POINT ( 'NONE',  ( 2.750000000000000888, 8.719000000000001194, 3.333750000000001990 ) ) ;
#2270 = AXIS2_PLACEMENT_3D ( 'NONE', #1879, #1961, #1273 ) ;
#2271 = VERTEX_POINT ( 'NONE', #1257 ) ;
#2272 = APPROVAL_DATE_TIME ( #5465, #3812 ) ;
#2273 = AXIS2_PLACEMENT_3D ( 'NONE', #7794, #1539, #1078 ) ;
#2274 = DIRECTION ( 'NONE',  ( -0.08785522444269551479, 0.000000000000000000, -0.9961332539063855185 ) ) ;
#2275 = CARTESIAN_POINT ( 'NONE',  ( 0.7333924044284368948, 4.107224863919222813, 7.960989307084956224 ) ) ;
#2276 = LINE ( 'NONE', #3547, #747 ) ;
#2277 = ADVANCED_FACE ( 'NONE', ( #6254 ), #641, .T. ) ;
#2278 = CIRCLE ( 'NONE', #8099, 0.2625000000000008438 ) ;
#2279 = ORIENTED_EDGE ( 'NONE', *, *, #8114, .T. ) ;
#2280 = ADVANCED_FACE ( 'NONE', ( #6712 ), #7343, .F. ) ;
#2281 = ORIENTED_EDGE ( 'NONE', *, *, #216, .T. ) ;
#2282 = CARTESIAN_POINT ( 'NONE',  ( -4.382879947506561180, 4.383999996532200960, 7.363250037317454755 ) ) ;
#2283 = FACE_OUTER_BOUND ( 'NONE', #5377, .T. ) ;
#2284 = VERTEX_POINT ( 'NONE', #676 ) ;
#2285 = APPROVAL_ROLE ( '' ) ;
#2286 = ADVANCED_FACE ( 'NONE', ( #3257 ), #5719, .T. ) ;
#2287 = LINE ( 'NONE', #5390, #1378 ) ;
#2288 = VECTOR ( 'NONE', #4955, 39.37007874015748143 ) ;
#2289 = LINE ( 'NONE', #4787, #5720 ) ;
#2290 = DATE_AND_TIME ( #2897, #6937 ) ;
#2291 = ORIENTED_EDGE ( 'NONE', *, *, #2446, .F. ) ;
#2292 = CIRCLE ( 'NONE', #44, 0.3124999879509117728 ) ;
#2293 = DIRECTION ( 'NONE',  ( 1.000000000000000000, 0.000000000000000000, 0.000000000000000000 ) ) ;
#2294 = LOCAL_TIME ( 0, 37, 23.00000000000000000, #2377 ) ;
#2295 = CIRCLE ( 'NONE', #6094, 1.074999999999999289 ) ;
#2296 = CARTESIAN_POINT ( 'NONE',  ( 3.562500000000000444, 1.000000000000000222, 2.975000000000000977 ) ) ;
#2297 = CLOSED_SHELL ( 'NONE', ( #7743, #6834, #5205, #4942, #102, #1595, #2042, #3429, #3498, #7738, #6763, #4867, #6159, #7423, #3671, #6696, #956, #8156, #5082 ) ) ;
#2298 = CC_DESIGN_APPROVAL ( #7190, ( #516 ) ) ;
#2299 = FACE_OUTER_BOUND ( 'NONE', #2313, .T. ) ;
#2300 = CARTESIAN_POINT ( 'NONE',  ( 3.875000000000001776, 1.000000000000000222, 7.750000000000002665 ) ) ;
#2301 = SECURITY_CLASSIFICATION_LEVEL ( 'unclassified' ) ;
#2302 = VERTEX_POINT ( 'NONE', #4523 ) ;
#2303 = CARTESIAN_POINT ( 'NONE',  ( -3.583510604133042232, 1.543025754838326824, -7.167021208266081800 ) ) ;
#2304 = AXIS2_PLACEMENT_3D ( 'NONE', #6993, #5795, #3258 ) ;
#2305 = EDGE_CURVE ( 'NONE', #231, #7215, #1103, .T. ) ;
#2306 = CARTESIAN_POINT ( 'NONE',  ( 1.625000000000000222, 5.113999999999999879, -2.749999999536767437 ) ) ;
#2307 = DIRECTION ( 'NONE',  ( 0.000000000000000000, 0.000000000000000000, 1.000000000000000000 ) ) ;
#2308 = DIRECTION ( 'NONE',  ( -0.000000000000000000, 1.000000000000000000, 0.000000000000000000 ) ) ;
#2309 = EDGE_CURVE ( 'NONE', #533, #442, #945, .T. ) ;
#2310 = DIRECTION ( 'NONE',  ( -0.000000000000000000, -1.000000000000000000, -0.000000000000000000 ) ) ;
#2311 = ORIENTED_EDGE ( 'NONE', *, *, #7444, .T. ) ;
#2312 = LINE ( 'NONE', #6002, #5928 ) ;
#2313 = EDGE_LOOP ( 'NONE', ( #2480, #2976, #7988 ) ) ;
#2314 = VECTOR ( 'NONE', #2643, 39.37007874015748143 ) ;
#2315 = AXIS2_PLACEMENT_3D ( 'NONE', #651, #3608, #6108 ) ;
#2316 = CC_DESIGN_DATE_AND_TIME_ASSIGNMENT ( #1871, #3939, ( #1197 ) ) ;
#2317 = CARTESIAN_POINT ( 'NONE',  ( -3.987046614173228143, 4.131461189141452550, 8.155839089539586695 ) ) ;
#2318 = DIRECTION ( 'NONE',  ( -0.000000000000000000, 0.000000000000000000, 1.000000000000000000 ) ) ;
#2319 = CARTESIAN_POINT ( 'NONE',  ( 0.000000000000000000, 2.500000000356088936, 0.000000000000000000 ) ) ;
#2320 = DIRECTION ( 'NONE',  ( -0.000000000000000000, -0.000000000000000000, 1.000000000000000000 ) ) ;
#2321 = AXIS2_PLACEMENT_3D ( 'NONE', #3266, #7687, #1915 ) ;
#2322 = ORIENTED_EDGE ( 'NONE', *, *, #6551, .T. ) ;
#2323 = CIRCLE ( 'NONE', #6242, 4.805751768934915624 ) ;
#2324 = PERSON_AND_ORGANIZATION_ROLE ( 'creator' ) ;
#2325 = CARTESIAN_POINT ( 'NONE',  ( 3.562500000000000444, -3.820994442221351629E-18, 2.612499999999998934 ) ) ;
#2326 = DIRECTION ( 'NONE',  ( 1.000000000000000000, 0.000000000000000000, 0.000000000000000000 ) ) ;
#2327 = ORIENTED_EDGE ( 'NONE', *, *, #8052, .F. ) ;
#2328 = DIRECTION ( 'NONE',  ( -0.000000000000000000, -0.000000000000000000, 1.000000000000000000 ) ) ;
#2329 = DIRECTION ( 'NONE',  ( -0.000000000000000000, 0.000000000000000000, -1.000000000000000000 ) ) ;
#2330 = DIRECTION ( 'NONE',  ( 0.000000000000000000, -0.000000000000000000, 1.000000000000000000 ) ) ;
#2331 = DIRECTION ( 'NONE',  ( -0.7071067811865474617, -0.7071067811865474617, -0.000000000000000000 ) ) ;
#2332 = ORIENTED_EDGE ( 'NONE', *, *, #6452, .F. ) ;
#2333 = APPROVAL_STATUS ( 'not_yet_approved' ) ;
#2334 = CARTESIAN_POINT ( 'NONE',  ( 3.987953385826771946, 3.674333370316267278, 8.782583289749323896 ) ) ;
#2335 = DATE_AND_TIME ( #7999, #2294 ) ;
#2336 = EDGE_LOOP ( 'NONE', ( #1617, #4325, #6298, #5291 ) ) ;
#2337 = CARTESIAN_POINT ( 'NONE',  ( -1.187500000000000222, 8.351123808764901568, 5.236250000000000959 ) ) ;
#2338 = LOCAL_TIME ( 0, 37, 23.00000000000000000, #110 ) ;
#2339 = EDGE_CURVE ( 'NONE', #6387, #4731, #4809, .T. ) ;
#2340 = DIRECTION ( 'NONE',  ( 0.000000000000000000, 0.000000000000000000, -1.000000000000000000 ) ) ;
#2341 = DIRECTION ( 'NONE',  ( 1.000000000000000000, -0.000000000000000000, 0.000000000000000000 ) ) ;
#2342 = CARTESIAN_POINT ( 'NONE',  ( 0.7335700383901263555, 2.500000000202698303, 2.908930215426092758 ) ) ;
#2343 = LENGTH_MEASURE_WITH_UNIT ( LENGTH_MEASURE( 0.02539999999999999897 ), #2951 );
#2344 = CARTESIAN_POINT ( 'NONE',  ( -1.500000000000000444, 5.414000000000000590, 2.749999998413802160 ) ) ;
#2345 = DATE_TIME_ROLE ( 'creation_date' ) ;
#2346 = EDGE_CURVE ( 'NONE', #5429, #7262, #2869, .T. ) ;
#2347 = ORIENTED_EDGE ( 'NONE', *, *, #1150, .F. ) ;
#2348 = CARTESIAN_POINT ( 'NONE',  ( -4.462046614173229564, 3.753500037802127043, 8.231249998505111520 ) ) ;
#2349 = DIRECTION ( 'NONE',  ( -0.000000000000000000, -1.000000000000000000, -0.000000000000000000 ) ) ;
#2350 = DIRECTION ( 'NONE',  ( -0.000000000000000000, -1.000000000000000000, -0.000000000000000000 ) ) ;
#2351 = DIRECTION ( 'NONE',  ( -0.7071067811865474617, -0.7071067811865474617, -0.000000000000000000 ) ) ;
#2352 = CARTESIAN_POINT ( 'NONE',  ( -1.388463899750249738E-31, 3.950000000000000178, 3.440250000000000696 ) ) ;
#2353 = CARTESIAN_POINT ( 'NONE',  ( 0.000000000000000000, 2.523992677165354248, 5.972081456692916568 ) ) ;
#2354 = EDGE_CURVE ( 'NONE', #2284, #2355, #1146, .T. ) ;
#2355 = VERTEX_POINT ( 'NONE', #7912 ) ;
#2356 = CARTESIAN_POINT ( 'NONE',  ( 0.000000000000000000, 7.974000000000001087, 3.323750000000001759 ) ) ;
#2357 = VERTEX_POINT ( 'NONE', #3488 ) ;
#2358 = LINE ( 'NONE', #7241, #1360 ) ;
#2359 = CARTESIAN_POINT ( 'NONE',  ( -3.687499989627468278, 1.000000000000000666, 3.874999999790589733 ) ) ;
#2360 = PRODUCT ( 'MAS-412', 'MAS-412', '', ( #8074 ) ) ;
#2361 = LINE ( 'NONE', #4933, #5670 ) ;
#2362 = VERTEX_POINT ( 'NONE', #3018 ) ;
#2363 = CALENDAR_DATE ( 2026, 8, 10 ) ;
#2364 = FACE_OUTER_BOUND ( 'NONE', #8053, .T. ) ;
#2365 = CALENDAR_DATE ( 2026, 8, 10 ) ;
#2366 =( REPRESENTATION_RELATIONSHIP ('NONE','NONE', #3256, #578 ) REPRESENTATION_RELATIONSHIP_WITH_TRANSFORMATION ( #3792 )SHAPE_REPRESENTATION_RELATIONSHIP( ) );
#2367 = EDGE_CURVE ( 'NONE', #5914, #3226, #6144, .T. ) ;
#2368 = CC_DESIGN_APPROVAL ( #1264, ( #3008 ) ) ;
#2369 = ORIENTED_EDGE ( 'NONE', *, *, #4131, .T. ) ;
#2370 = CARTESIAN_POINT ( 'NONE',  ( -3.343750000000002220, 1.750000000000000444, -0.5624999991015005030 ) ) ;
#2371 = CARTESIAN_POINT ( 'NONE',  ( 0.000000000000000000, 7.964000000000000412, 0.000000000000000000 ) ) ;
#2372 = DIRECTION ( 'NONE',  ( -1.000000000000000000, 0.000000000000000000, -0.000000000000000000 ) ) ;
#2373 = ORIENTED_EDGE ( 'NONE', *, *, #2768, .T. ) ;
#2374 = PERSON_AND_ORGANIZATION_ROLE ( 'design_supplier' ) ;
#2375 = FACE_OUTER_BOUND ( 'NONE', #7389, .T. ) ;
#2376 = CARTESIAN_POINT ( 'NONE',  ( -0.3381868542694876911, 5.218913450356295058, -5.108750000000003233 ) ) ;
#2377 = COORDINATED_UNIVERSAL_TIME_OFFSET ( 0, 0, .AHEAD. ) ;
#2378 = CC_DESIGN_DATE_AND_TIME_ASSIGNMENT ( #4242, #1678, ( #3944 ) ) ;
#2379 = ADVANCED_FACE ( 'NONE', ( #3525 ), #1068, .T. ) ;
#2380 = DIRECTION ( 'NONE',  ( -0.000000000000000000, 0.7071067811865474617, 0.7071067811865474617 ) ) ;
#2381 = PLANE ( 'NONE',  #3747 ) ;
#2382 = ORIENTED_EDGE ( 'NONE', *, *, #5480, .F. ) ;
#2383 = EDGE_CURVE ( 'NONE', #6055, #2284, #6023, .T. ) ;
#2384 = FACE_OUTER_BOUND ( 'NONE', #7432, .T. ) ;
#2385 = PERSON_AND_ORGANIZATION ( #7862, #8117 ) ;
#2386 = ORIENTED_EDGE ( 'NONE', *, *, #7832, .T. ) ;
#2387 = ADVANCED_FACE ( 'NONE', ( #2900 ), #446, .T. ) ;
#2388 = CARTESIAN_POINT ( 'NONE',  ( -3.875000000000002220, 1.000000000000000222, 4.745506346695996852E-16 ) ) ;
#2389 = ORIENTED_EDGE ( 'NONE', *, *, #548, .T. ) ;
#2390 = DIRECTION ( 'NONE',  ( -0.000000000000000000, 1.000000000000000000, -0.000000000000000000 ) ) ;
#2391 = DIRECTION ( 'NONE',  ( 0.000000000000000000, 1.000000000000000000, 0.000000000000000000 ) ) ;
#2392 = VERTEX_POINT ( 'NONE', #6616 ) ;
#2393 = CARTESIAN_POINT ( 'NONE',  ( -3.987046614173228587, 3.950000015938371689, 8.231249998505111520 ) ) ;
#2394 = EDGE_LOOP ( 'NONE', ( #3021, #3642, #3652, #8118, #4951, #1106 ) ) ;
#2395 = EDGE_CURVE ( 'NONE', #5001, #533, #7467, .T. ) ;
#2396 = EDGE_CURVE ( 'NONE', #2706, #6912, #2944, .T. ) ;
#2397 = CARTESIAN_POINT ( 'NONE',  ( 3.987953385826771946, 4.098527760758083893, 8.101886876862897324 ) ) ;
#2398 = CARTESIAN_POINT ( 'NONE',  ( -1.161591181102362702, 3.052477677165355008, -4.271824881889764391 ) ) ;
#2399 = CARTESIAN_POINT ( 'NONE',  ( -2.750000000000000888, 7.974000000000001087, 3.813750000000002416 ) ) ;
#2400 = CARTESIAN_POINT ( 'NONE',  ( 2.750000000000000888, 7.974000000000001087, 3.813750000000002416 ) ) ;
#2401 = ORIENTED_EDGE ( 'NONE', *, *, #6398, .F. ) ;
#2402 = DATE_AND_TIME ( #7593, #3583 ) ;
#2403 = LINE ( 'NONE', #6091, #4264 ) ;
#2404 = VECTOR ( 'NONE', #8019, 39.37007874015748854 ) ;
#2405 = CIRCLE ( 'NONE', #7801, 3.343750000000001332 ) ;
#2406 = LOCAL_TIME ( 0, 37, 23.00000000000000000, #3555 ) ;
#2407 = EDGE_CURVE ( 'NONE', #3267, #4783, #3245, .T. ) ;
#2408 = ORIENTED_EDGE ( 'NONE', *, *, #849, .F. ) ;
#2409 = CIRCLE ( 'NONE', #3954, 0.3625000000000019318 ) ;
#2410 = DIRECTION ( 'NONE',  ( 1.000000000000000000, 0.000000000000000000, 0.000000000000000000 ) ) ;
#2411 = VECTOR ( 'NONE', #2307, 39.37007874015748143 ) ;
#2412 = CARTESIAN_POINT ( 'NONE',  ( -4.462046614173230452, 4.225666661560478765, 8.231249998505111520 ) ) ;
#2413 = VERTEX_POINT ( 'NONE', #4740 ) ;
#2414 = APPROVAL_ROLE ( '' ) ;
#2415 = DIRECTION ( 'NONE',  ( 0.000000000000000000, -0.000000000000000000, 1.000000000000000000 ) ) ;
#2416 = CARTESIAN_POINT ( 'NONE',  ( -0.2965954673551001730, 5.229263513284051257, -5.108749999999999680 ) ) ;
#2417 = CALENDAR_DATE ( 2026, 8, 10 ) ;
#2418 = DIRECTION ( 'NONE',  ( -1.000000000000000000, 0.000000000000000000, 0.000000000000000000 ) ) ;
#2419 = VECTOR ( 'NONE', #3912, 39.37007874015748143 ) ;
#2420 = CARTESIAN_POINT ( 'NONE',  ( 0.000000000000000000, 0.000000000000000000, 4.323750000000001315 ) ) ;
#2421 = APPROVAL ( #1293, 'UNSPECIFIED' ) ;
#2422 = VECTOR ( 'NONE', #3809, 39.37007874015748854 ) ;
#2423 = CARTESIAN_POINT ( 'NONE',  ( 3.791570907149167446, 1.000000000000000222, 0.7997593697006841751 ) ) ;
#2424 = ORIENTED_EDGE ( 'NONE', *, *, #5697, .T. ) ;
#2425 = CARTESIAN_POINT ( 'NONE',  ( -0.7457411423250318583, 4.032391550759110821, 8.533409342498828210 ) ) ;
#2426 = AXIS2_PLACEMENT_3D ( 'NONE', #4239, #6053, #3553 ) ;
#2427 =( CONVERSION_BASED_UNIT ( 'INCH', #7958 ) LENGTH_UNIT ( ) NAMED_UNIT ( #7017 ) );
#2428 = DIRECTION ( 'NONE',  ( -0.3026345437601030697, -0.000000000000000000, -0.9531066744720204653 ) ) ;
#2429 = MECHANICAL_CONTEXT ( 'NONE', #6515, 'mechanical' ) ;
#2430 = ORIENTED_EDGE ( 'NONE', *, *, #2367, .T. ) ;
#2431 = CARTESIAN_POINT ( 'NONE',  ( 2.740000000000000657, 7.964000000000000412, 3.813750000000002416 ) ) ;
#2432 = CIRCLE ( 'NONE', #591, 5.349138356872925826 ) ;
#2433 = PRODUCT_DEFINITION_SHAPE ( 'NONE', 'NONE',  #516 ) ;
#2434 = ORIENTED_EDGE ( 'NONE', *, *, #3285, .T. ) ;
#2435 = LINE ( 'NONE', #5491, #1886 ) ;
#2436 = FACE_OUTER_BOUND ( 'NONE', #5782, .T. ) ;
#2437 = AXIS2_PLACEMENT_3D ( 'NONE', #3261, #3181, #1301 ) ;
#2438 = VECTOR ( 'NONE', #5967, 39.37007874015748143 ) ;
#2439 = VERTEX_POINT ( 'NONE', #11 ) ;
#2440 = CARTESIAN_POINT ( 'NONE',  ( -0.6827599196736726661, 3.639582871947503850, 8.272753927050759515 ) ) ;
#2441 = ADVANCED_FACE ( 'NONE', ( #6304 ), #3718, .T. ) ;
#2442 = ORIENTED_EDGE ( 'NONE', *, *, #8079, .F. ) ;
#2443 = EDGE_CURVE ( 'NONE', #7113, #2476, #4411, .T. ) ;
#2444 = PERSON ( 'NAUO-PER1', 'UNSPECIFIED', 'UNSPECIFIED', ('UNSPECIFIED'), ('UNSPECIFIED'), ('UNSPECIFIED') ) ;
#2445 = AXIS2_PLACEMENT_3D ( 'NONE', #4679, #7335, #4646 ) ;
#2446 = EDGE_CURVE ( 'NONE', #3785, #47, #6218, .T. ) ;
#2447 = CARTESIAN_POINT ( 'NONE',  ( 3.987953385826772834, 4.126152250297301372, 8.143725961102258992 ) ) ;
#2448 = CARTESIAN_POINT ( 'NONE',  ( 2.750000000000000888, 8.719000000000001194, 3.813750000000002416 ) ) ;
#2449 = CARTESIAN_POINT ( 'NONE',  ( -2.750000000000000444, 8.719000000000002970, 3.833750000000001545 ) ) ;
#2450 = CARTESIAN_POINT ( 'NONE',  ( -1.198957880828181333, 2.500000000000000000, -2.750000000000000444 ) ) ;
#2451 = CARTESIAN_POINT ( 'NONE',  ( 0.7335700393700786970, 2.500000000000000444, 2.909883779527559611 ) ) ;
#2452 = VERTEX_POINT ( 'NONE', #5603 ) ;
#2453 = CALENDAR_DATE ( 2026, 8, 10 ) ;
#2454 = CARTESIAN_POINT ( 'NONE',  ( 1.249999999999999556, 3.950000000000000178, 3.691250000234376660 ) ) ;
#2455 = VECTOR ( 'NONE', #3064, 39.37007874015748143 ) ;
#2456 = VECTOR ( 'NONE', #4425, 39.37007874015748143 ) ;
#2457 = CIRCLE ( 'NONE', #7318, 3.000000000518587839 ) ;
#2458 = DIRECTION ( 'NONE',  ( -1.000000000000000000, 0.000000000000000000, -0.000000000000000000 ) ) ;
#2459 = VECTOR ( 'NONE', #5675, 39.37007874015748143 ) ;
#2460 = CARTESIAN_POINT ( 'NONE',  ( -1.187500000000000000, 5.969165905511811587, 6.858307716535433585 ) ) ;
#2461 = CARTESIAN_POINT ( 'NONE',  ( 1.187500000000000444, 8.523567380006621619, 4.820336057633928029 ) ) ;
#2462 = EDGE_LOOP ( 'NONE', ( #7552, #141, #787, #2032 ) ) ;
#2463 = PERSON_AND_ORGANIZATION ( #7862, #8117 ) ;
#2464 = CARTESIAN_POINT ( 'NONE',  ( 4.462953385826772923, 3.674333370316267278, 8.782583289749323896 ) ) ;
#2465 = CONTEXT_DEPENDENT_SHAPE_REPRESENTATION ( #6855, #3831 ) ;
#2466 = PLANE ( 'NONE',  #3574 ) ;
#2467 = CARTESIAN_POINT ( 'NONE',  ( 1.124999999999999556, 3.950000000000000178, 6.956250000000000711 ) ) ;
#2468 = CARTESIAN_POINT ( 'NONE',  ( 0.000000000000000000, 3.950000000000000178, 8.981250000000001066 ) ) ;
#2469 = ORIENTED_EDGE ( 'NONE', *, *, #5327, .T. ) ;
#2470 = CARTESIAN_POINT ( 'NONE',  ( -0.7456179150311872394, 4.031565731729908286, 7.929405685993585529 ) ) ;
#2471 = DIRECTION ( 'NONE',  ( 0.000000000000000000, 0.000000000000000000, -1.000000000000000000 ) ) ;
#2472 = APPROVAL_STATUS ( 'not_yet_approved' ) ;
#2473 = VERTEX_POINT ( 'NONE', #8167 ) ;
#2474 = CARTESIAN_POINT ( 'NONE',  ( 4.470366332363715500, 1.365923996832131609E-16, 2.937534001674282358 ) ) ;
#2475 = CC_DESIGN_DATE_AND_TIME_ASSIGNMENT ( #3918, #4547, ( #4146 ) ) ;
#2476 = VERTEX_POINT ( 'NONE', #58 ) ;
#2477 = LOCAL_TIME ( 0, 37, 23.00000000000000000, #2508 ) ;
#2478 = CARTESIAN_POINT ( 'NONE',  ( 2.740000000000001545, 8.729000000000002757, 4.313750000000002416 ) ) ;
#2479 =( CONVERSION_BASED_UNIT ( 'INCH', #2010 ) LENGTH_UNIT ( ) NAMED_UNIT ( #5699 ) );
#2480 = ORIENTED_EDGE ( 'NONE', *, *, #7987, .T. ) ;
#2481 = DIRECTION ( 'NONE',  ( -1.000000000000000000, 0.000000000000000000, 0.000000000000000000 ) ) ;
#2482 = ORIENTED_EDGE ( 'NONE', *, *, #3533, .F. ) ;
#2483 = PRODUCT_DEFINITION ( 'UNKNOWN', '', #1491, #2756 ) ;
#2484 = CARTESIAN_POINT ( 'NONE',  ( 3.987953385826772390, 4.136475903844373470, 8.169134493240660433 ) ) ;
#2485 = CARTESIAN_POINT ( 'NONE',  ( 1.986718228346456838, 3.767850944881891095, -4.887177007874016432 ) ) ;
#2486 = EDGE_CURVE ( 'NONE', #4681, #2413, #5185, .T. ) ;
#2487 = FACE_OUTER_BOUND ( 'NONE', #219, .T. ) ;
#2488 = EDGE_CURVE ( 'NONE', #8018, #7866, #3224, .T. ) ;
#2489 = ORIENTED_EDGE ( 'NONE', *, *, #3708, .T. ) ;
#2490 = APPROVAL_DATE_TIME ( #3783, #2421 ) ;
#2491 = CARTESIAN_POINT ( 'NONE',  ( 3.987953385826773278, 3.792944682096142550, 8.350119983549243230 ) ) ;
#2492 = ORIENTED_EDGE ( 'NONE', *, *, #2309, .T. ) ;
#2493 = EDGE_CURVE ( 'NONE', #5429, #2620, #6798, .T. ) ;
#2494 = CARTESIAN_POINT ( 'NONE',  ( 1.187500000000000444, 7.436775081392276832, 4.083473622006301262 ) ) ;
#2495 = ORIENTED_EDGE ( 'NONE', *, *, #5261, .F. ) ;
#2496 = CALENDAR_DATE ( 2026, 8, 10 ) ;
#2497 = CARTESIAN_POINT ( 'NONE',  ( 4.067120052493439886, 3.516000035344543306, 8.231249998505111520 ) ) ;
#2498 = COORDINATED_UNIVERSAL_TIME_OFFSET ( 0, 0, .AHEAD. ) ;
#2499 = DIRECTION ( 'NONE',  ( 0.000000000000000000, 0.000000000000000000, -1.000000000000000000 ) ) ;
#2500 = EDGE_CURVE ( 'NONE', #3620, #3785, #2177, .T. ) ;
#2501 = CARTESIAN_POINT ( 'NONE',  ( 3.296097361251832503, 1.749999999892448477, 0.5624999982029994516 ) ) ;
#2502 = CARTESIAN_POINT ( 'NONE',  ( 1.625000000000000222, 2.500000000000000000, -2.521780125229002412 ) ) ;
#2503 = DIRECTION ( 'NONE',  ( -0.000000000000000000, -0.000000000000000000, 1.000000000000000000 ) ) ;
#2504 = VERTEX_POINT ( 'NONE', #6875 ) ;
#2505 = CARTESIAN_POINT ( 'NONE',  ( -0.6818077110526902240, 4.262471192484426297, 8.210173163913728089 ) ) ;
#2506 = CARTESIAN_POINT ( 'NONE',  ( -1.187500000000000444, 4.186788071090408181, 6.858307717089314970 ) ) ;
#2507 = LINE ( 'NONE', #3121, #1019 ) ;
#2508 = COORDINATED_UNIVERSAL_TIME_OFFSET ( 0, 0, .AHEAD. ) ;
#2509 = ORIENTED_EDGE ( 'NONE', *, *, #2395, .T. ) ;
#2510 = CARTESIAN_POINT ( 'NONE',  ( -1.172489672300577768, 1.000000000000000888, -3.693357952253316423 ) ) ;
#2511 = PLANE ( 'NONE',  #314 ) ;
#2512 = SHAPE_REPRESENTATION_RELATIONSHIP ( 'NONE' , 'NONE' ,  #4813, #659 ) ;
#2513 = ORIENTED_EDGE ( 'NONE', *, *, #4877, .T. ) ;
#2514 = ORIENTED_EDGE ( 'NONE', *, *, #1538, .F. ) ;
#2515 = VERTEX_POINT ( 'NONE', #6954 ) ;
#2516 = CARTESIAN_POINT ( 'NONE',  ( -0.2278784911965701654, 2.340730451631669151, -3.064708773258130847 ) ) ;
#2517 = APPROVAL ( #8091, 'UNSPECIFIED' ) ;
#2518 = CARTESIAN_POINT ( 'NONE',  ( 1.213899189620355035, 3.445445541707729653, -5.108749999999997904 ) ) ;
#2519 = CARTESIAN_POINT ( 'NONE',  ( -1.500000000000000444, 5.113999999999999879, 2.749999998413802160 ) ) ;
#2520 = ORIENTED_EDGE ( 'NONE', *, *, #776, .T. ) ;
#2521 = COORDINATED_UNIVERSAL_TIME_OFFSET ( 0, 0, .AHEAD. ) ;
#2522 = CARTESIAN_POINT ( 'NONE',  ( 3.987953385826772834, 3.753500037802127931, 8.243740188834737026 ) ) ;
#2523 = CARTESIAN_POINT ( 'NONE',  ( -0.7499999999999993339, 3.929104627039255782, 8.543750000000002842 ) ) ;
#2524 = ORIENTED_EDGE ( 'NONE', *, *, #2537, .F. ) ;
#2525 = EDGE_CURVE ( 'NONE', #6945, #6736, #3059, .T. ) ;
#2526 = CARTESIAN_POINT ( 'NONE',  ( -2.749999999999999556, 7.339000000000001300, 3.161250000000001670 ) ) ;
#2527 = AXIS2_PLACEMENT_3D ( 'NONE', #1081, #2962, #4846 ) ;
#2528 = VERTEX_POINT ( 'NONE', #6261 ) ;
#2529 = PERSON_AND_ORGANIZATION ( #7862, #8117 ) ;
#2530 = VECTOR ( 'NONE', #7240, 39.37007874015748143 ) ;
#2531 = DIRECTION ( 'NONE',  ( -0.000000000000000000, 1.000000000000000000, -0.000000000000000000 ) ) ;
#2532 = DIRECTION ( 'NONE',  ( -0.000000000000000000, 1.000000000000000000, -0.000000000000000000 ) ) ;
#2533 = LOCAL_TIME ( 0, 37, 23.00000000000000000, #5251 ) ;
#2534 = APPROVAL_ROLE ( '' ) ;
#2535 = DIRECTION ( 'NONE',  ( -0.000000000000000000, -0.000000000000000000, 1.000000000000000000 ) ) ;
#2536 = EDGE_CURVE ( 'NONE', #691, #5594, #7375, .T. ) ;
#2537 = EDGE_CURVE ( 'NONE', #1938, #1701, #4008, .T. ) ;
#2538 = AXIS2_PLACEMENT_3D ( 'NONE', #1696, #6585, #957 ) ;
#2539 = LOCAL_TIME ( 0, 37, 23.00000000000000000, #5296 ) ;
#2540 = CARTESIAN_POINT ( 'NONE',  ( -3.987046614173228143, 3.815844187783087094, 8.087511858761828876 ) ) ;
#2541 = DIRECTION ( 'NONE',  ( 0.000000000000000000, 0.000000000000000000, 1.000000000000000000 ) ) ;
#2542 = EDGE_CURVE ( 'NONE', #3034, #539, #7717, .T. ) ;
#2543 = CARTESIAN_POINT ( 'NONE',  ( 0.000000000000000000, 1.750000000000000444, 2.693920355039552791E-42 ) ) ;
#2544 = VERTEX_POINT ( 'NONE', #1430 ) ;
#2545 = CARTESIAN_POINT ( 'NONE',  ( -4.382879947506561180, 4.383999996532200960, 9.099249959692771839 ) ) ;
#2546 = CARTESIAN_POINT ( 'NONE',  ( -1.187500000000000444, 4.734451501383331262, 5.775979225330971190 ) ) ;
#2547 = VECTOR ( 'NONE', #1786, 39.37007874015748143 ) ;
#2548 = DATE_TIME_ROLE ( 'creation_date' ) ;
#2549 = VERTEX_POINT ( 'NONE', #2735 ) ;
#2550 = DIRECTION ( 'NONE',  ( 0.000000000000000000, 0.000000000000000000, -1.000000000000000000 ) ) ;
#2551 = EDGE_CURVE ( 'NONE', #5362, #2620, #3390, .T. ) ;
#2552 = CIRCLE ( 'NONE', #39, 2.845000000000001528 ) ;
#2553 = DIRECTION ( 'NONE',  ( -0.000000000000000000, -0.000000000000000000, 1.000000000000000000 ) ) ;
#2554 = CARTESIAN_POINT ( 'NONE',  ( 2.750000000000000444, 7.964000000000000412, 3.833750000000001545 ) ) ;
#2555 = ORIENTED_EDGE ( 'NONE', *, *, #943, .F. ) ;
#2556 = ORIENTED_EDGE ( 'NONE', *, *, #6831, .T. ) ;
#2557 = EDGE_CURVE ( 'NONE', #6895, #3907, #5692, .T. ) ;
#2558 = CARTESIAN_POINT ( 'NONE',  ( 3.987953385826772390, 3.764952780855910675, 8.164838062276935204 ) ) ;
#2559 = CARTESIAN_POINT ( 'NONE',  ( 0.8008852451031778230, 4.990709419004156544, -5.108750000000001457 ) ) ;
#2560 = CARTESIAN_POINT ( 'NONE',  ( 3.224046039892453308, 0.9999999999999642508, -2.215849741979416088 ) ) ;
#2561 = ORIENTED_EDGE ( 'NONE', *, *, #5261, .T. ) ;
#2562 = PERSON_AND_ORGANIZATION ( #7862, #8117 ) ;
#2563 = CARTESIAN_POINT ( 'NONE',  ( 3.987953385826772834, 3.760254621899925542, 8.283055230728429308 ) ) ;
#2564 = DIMENSIONAL_EXPONENTS ( 1.000000000000000000, 0.000000000000000000, 0.000000000000000000, 0.000000000000000000, 0.000000000000000000, 0.000000000000000000, 0.000000000000000000 ) ;
#2565 = ORIENTED_EDGE ( 'NONE', *, *, #2731, .T. ) ;
#2566 = AXIS2_PLACEMENT_3D ( 'NONE', #7796, #6412, #5755 ) ;
#2567 = CC_DESIGN_PERSON_AND_ORGANIZATION_ASSIGNMENT ( #3388, #3347, ( #1197 ) ) ;
#2568 = EDGE_CURVE ( 'NONE', #6635, #212, #3302, .T. ) ;
#2569 = DIRECTION ( 'NONE',  ( 1.000000000000000000, 0.000000000000000000, 0.000000000000000000 ) ) ;
#2570 = DIRECTION ( 'NONE',  ( -0.000000000000000000, -1.000000000000000000, 0.000000000000000000 ) ) ;
#2571 = CARTESIAN_POINT ( 'NONE',  ( -3.791570908345035740, 1.365923996832131609E-16, 0.7997593681799639587 ) ) ;
#2572 = AXIS2_PLACEMENT_3D ( 'NONE', #6920, #1272, #3721 ) ;
#2573 = ORIENTED_EDGE ( 'NONE', *, *, #6497, .T. ) ;
#2574 = CALENDAR_DATE ( 2026, 8, 10 ) ;
#2575 = DIRECTION ( 'NONE',  ( 1.000000000000000000, 0.000000000000000000, 0.000000000000000000 ) ) ;
#2576 = FACE_OUTER_BOUND ( 'NONE', #6657, .T. ) ;
#2577 = AXIS2_PLACEMENT_3D ( 'NONE', #395, #7341, #5381 ) ;
#2578 = CARTESIAN_POINT ( 'NONE',  ( -3.987046614173228143, 3.874591561940378792, 8.049793446537691466 ) ) ;
#2579 = CARTESIAN_POINT ( 'NONE',  ( 3.479221556377631263E-16, 1.664000000000000368, -2.841000000000000636 ) ) ;
#2580 = CARTESIAN_POINT ( 'NONE',  ( -3.987046614173228587, 3.674333370316265945, 8.231249998505111520 ) ) ;
#2581 = ORIENTED_EDGE ( 'NONE', *, *, #4250, .T. ) ;
#2582 = DIRECTION ( 'NONE',  ( 0.000000000000000000, 0.000000000000000000, 1.000000000000000000 ) ) ;
#2583 = CARTESIAN_POINT ( 'NONE',  ( 2.750000000000000444, 7.541160346212514298, 3.714531354832316445 ) ) ;
#2584 = CARTESIAN_POINT ( 'NONE',  ( -1.187500000000000666, 4.849020343544465206, 5.300059296325243530 ) ) ;
#2585 = EDGE_CURVE ( 'NONE', #1666, #5045, #4112, .T. ) ;
#2586 = APPROVAL_DATE_TIME ( #782, #1208 ) ;
#2587 = AXIS2_PLACEMENT_3D ( 'NONE', #4089, #7408, #1728 ) ;
#2588 = ORIENTED_EDGE ( 'NONE', *, *, #3163, .T. ) ;
#2589 = CARTESIAN_POINT ( 'NONE',  ( -2.078417272059708142E-11, 3.950000000000000178, 2.749999998413802160 ) ) ;
#2590 = ADVANCED_FACE ( 'NONE', ( #5925 ), #5890, .F. ) ;
#2591 = B_SPLINE_CURVE_WITH_KNOTS ( 'NONE', 3,
 ( #5627, #2522, #45, #2563, #87, #8155, #5054, #3860, #7594, #1947, #6371, #6944, #2602, #7669, #2491, #3253, #5092, #2023, #4519, #7631, #5757, #125, #1416, #5210, #6588, #4058, #5791, #220, #1455, #4640, #5329, #300, #7154, #5290, #171, #2145, #7844, #7195, #6504, #2804, #2685, #962, #5173, #2193, #7716, #4021, #6548, #2722, #2108, #919, #1616, #1541, #2070, #4561, #7069, #4680, #7114, #3932, #3456, #5958, #3417, #5912, #877, #5880, #6457, #1576 ),
 .UNSPECIFIED., .F., .F.,
 ( 4, 1, 1, 1, 1, 2, 2, 1, 2, 2, 2, 1, 2, 2, 1, 1, 1, 2, 2, 2, 1, 1, 1, 1, 2, 2, 1, 2, 2, 2, 1, 2, 2, 1, 1, 2, 2, 1, 1, 1, 2, 2, 4 ),
 ( 0.000000000000000000, 0.06249999999999043820, 0.09374999999998293032, 0.1093749999999795441, 0.1171874999999774070, 0.1210937499999789196, 0.1249999999999804323, 0.1562499999999877598, 0.1718749999999885369, 0.1874999999999892863, 0.2499999999999923950, 0.2812499999999912847, 0.2968749999999907296, 0.3124999999999901745, 0.3437499999999868994, 0.3593749999999852340, 0.3671874999999832356, 0.3710937499999822364, 0.3749999999999812372, 0.4999999999999621414, 0.5624999999999512612, 0.5937499999999463762, 0.6093749999999424904, 0.6171874999999398259, 0.6210937499999392708, 0.6249999999999388267, 0.6562499999999519273, 0.6718749999999595879, 0.6874999999999673594, 0.7499999999999937828, 0.7812500000000061062, 0.7968750000000112133, 0.8125000000000162093, 0.8437500000000262013, 0.8593750000000284217, 0.8671875000000294209, 0.8750000000000304201, 0.9062500000000217604, 0.9218750000000145439, 0.9296875000000108802, 0.9335937500000087708, 0.9375000000000065503, 1.000000000000000000 ),
 .UNSPECIFIED. ) ;
#2592 = DIRECTION ( 'NONE',  ( 0.000000000000000000, 0.000000000000000000, -1.000000000000000000 ) ) ;
#2593 = DIRECTION ( 'NONE',  ( 1.000000000000000000, 0.000000000000000000, 0.000000000000000000 ) ) ;
#2594 = CARTESIAN_POINT ( 'NONE',  ( 3.791570907149167002, 1.000000000000000222, 0.7997593697006841751 ) ) ;
#2595 = ORIENTED_EDGE ( 'NONE', *, *, #4641, .T. ) ;
#2596 = EDGE_LOOP ( 'NONE', ( #6204, #1487, #1238, #3458, #3246, #117, #4780, #5599 ) ) ;
#2597 = CARTESIAN_POINT ( 'NONE',  ( 3.987953385826773278, 3.769836505190169884, 8.152788242568149712 ) ) ;
#2598 = EDGE_CURVE ( 'NONE', #5045, #4460, #6562, .T. ) ;
#2599 = CARTESIAN_POINT ( 'NONE',  ( 0.8651000694493629073, 2.962007182104931413, -5.108749999999997904 ) ) ;
#2600 = DIRECTION ( 'NONE',  ( 0.000000000000000000, 0.000000000000000000, 1.000000000000000000 ) ) ;
#2601 = ORIENTED_EDGE ( 'NONE', *, *, #3921, .T. ) ;
#2602 = CARTESIAN_POINT ( 'NONE',  ( 3.987953385826771058, 3.781968321578446979, 8.333174882269297257 ) ) ;
#2603 = ORIENTED_EDGE ( 'NONE', *, *, #3392, .F. ) ;
#2604 = PRODUCT_DEFINITION_SHAPE ( 'NONE', 'NONE',  #8195 ) ;
#2605 = CARTESIAN_POINT ( 'NONE',  ( 2.349999998660270872, 3.550000000000001155, 0.3883559095726499266 ) ) ;
#2606 = DIRECTION ( 'NONE',  ( -1.000000000000000000, 0.000000000000000000, -0.000000000000000000 ) ) ;
#2607 = CARTESIAN_POINT ( 'NONE',  ( 2.150000000000000799, 5.025000000000000355, 3.742515787401574645 ) ) ;
#2608 = ORIENTED_EDGE ( 'NONE', *, *, #252, .F. ) ;
#2609 = APPROVAL_STATUS ( 'not_yet_approved' ) ;
#2610 = DIRECTION ( 'NONE',  ( -0.000000000000000000, 1.000000000000000000, 0.000000000000000000 ) ) ;
#2611 = PERSON_AND_ORGANIZATION_ROLE ( 'classification_officer' ) ;
#2612 = CARTESIAN_POINT ( 'NONE',  ( -2.537500000000000533, 1.664000000000000368, 0.2625000000000008438 ) ) ;
#2613 = DIRECTION ( 'NONE',  ( 1.000000000000000000, 0.000000000000000000, 0.000000000000000000 ) ) ;
#2614 = CARTESIAN_POINT ( 'NONE',  ( 0.000000000000000000, 5.539742775656026019, 3.998660959628785871 ) ) ;
#2615 = DIMENSIONAL_EXPONENTS ( 1.000000000000000000, 0.000000000000000000, 0.000000000000000000, 0.000000000000000000, 0.000000000000000000, 0.000000000000000000, 0.000000000000000000 ) ;
#2616 = ORIENTED_EDGE ( 'NONE', *, *, #6285, .T. ) ;
#2617 = CARTESIAN_POINT ( 'NONE',  ( 3.987953385826772390, 3.950000015938371689, 8.231249998505111520 ) ) ;
#2618 = CARTESIAN_POINT ( 'NONE',  ( 1.500000000000000444, 5.113999999999999879, 0.000000000000000000 ) ) ;
#2619 = CARTESIAN_POINT ( 'NONE',  ( -3.987046614173229475, 3.898199183958024783, 8.420997134034164944 ) ) ;
#2620 = VERTEX_POINT ( 'NONE', #7814 ) ;
#2621 = PLANE ( 'NONE',  #6073 ) ;
#2622 = CC_DESIGN_DATE_AND_TIME_ASSIGNMENT ( #555, #3790, ( #4922 ) ) ;
#2623 = CARTESIAN_POINT ( 'NONE',  ( -2.750000000000000444, 7.339000000000003077, 4.175863149606300340 ) ) ;
#2624 = CALENDAR_DATE ( 2026, 8, 10 ) ;
#2625 = CARTESIAN_POINT ( 'NONE',  ( 2.750000000000002665, 7.963999999999999524, 2.411250000000000338 ) ) ;
#2626 = ORIENTED_EDGE ( 'NONE', *, *, #4363, .F. ) ;
#2627 = DIRECTION ( 'NONE',  ( 0.000000000000000000, 0.000000000000000000, -1.000000000000000000 ) ) ;
#2628 = CARTESIAN_POINT ( 'NONE',  ( -4.936857409062767316E-17, 2.875000000000000444, 3.440250000000001140 ) ) ;
#2629 = ADVANCED_FACE ( 'NONE', ( #4693 ), #7209, .F. ) ;
#2630 = APPROVAL_DATE_TIME ( #5663, #3215 ) ;
#2631 = FACE_OUTER_BOUND ( 'NONE', #4895, .T. ) ;
#2632 = APPROVAL_PERSON_ORGANIZATION ( #6444, #5566, #4048 ) ;
#2633 = DIRECTION ( 'NONE',  ( 0.7071067811865474617, 0.7071067811865474617, 0.000000000000000000 ) ) ;
#2634 = EDGE_CURVE ( 'NONE', #3785, #674, #2457, .T. ) ;
#2635 = LINE ( 'NONE', #5086, #323 ) ;
#2636 = ORIENTED_EDGE ( 'NONE', *, *, #1427, .F. ) ;
#2637 = ORIENTED_EDGE ( 'NONE', *, *, #4052, .T. ) ;
#2638 = ADVANCED_FACE ( 'NONE', ( #1553 ), #3391, .T. ) ;
#2639 = CARTESIAN_POINT ( 'NONE',  ( -2.740000000000000657, 7.974000000000001087, 3.823750000000002647 ) ) ;
#2640 = CARTESIAN_POINT ( 'NONE',  ( 1.205291313024512867, 4.469991316918233260, -5.108749999999997904 ) ) ;
#2641 = CARTESIAN_POINT ( 'NONE',  ( 0.000000000000000000, 3.950000000000000178, 3.691250000234376660 ) ) ;
#2642 = ORIENTED_EDGE ( 'NONE', *, *, #3917, .T. ) ;
#2643 = DIRECTION ( 'NONE',  ( 1.000000000000000000, 0.000000000000000000, -0.000000000000000000 ) ) ;
#2644 = CARTESIAN_POINT ( 'NONE',  ( 1.462953684461641091, 1.000000000000000888, 3.588229578933126440 ) ) ;
#2645 = EDGE_LOOP ( 'NONE', ( #7697, #886, #5653, #1928 ) ) ;
#2646 = ADVANCED_FACE ( 'NONE', ( #2854 ), #7248, .T. ) ;
#2647 = EDGE_CURVE ( 'NONE', #6784, #6962, #6426, .T. ) ;
#2648 = DIRECTION ( 'NONE',  ( 1.000000000000000000, 0.000000000000000000, 0.000000000000000000 ) ) ;
#2649 = PLANE ( 'NONE',  #199 ) ;
#2650 = CARTESIAN_POINT ( 'NONE',  ( 4.462953385826771147, 4.146499994075096396, 7.838250042231665660 ) ) ;
#2651 = ORIENTED_EDGE ( 'NONE', *, *, #7420, .F. ) ;
#2652 = PERSON_AND_ORGANIZATION_ROLE ( 'design_owner' ) ;
#2653 = CYLINDRICAL_SURFACE ( 'NONE', #195, 1.249999999999999556 ) ;
#2654 = DATE_AND_TIME ( #188, #4587 ) ;
#2655 = CARTESIAN_POINT ( 'NONE',  ( 0.7417920657368231030, 3.838932697565026864, 7.938974592032494115 ) ) ;
#2656 = DIRECTION ( 'NONE',  ( 0.000000000000000000, 1.000000000000000000, 0.000000000000000000 ) ) ;
#2657 = CARTESIAN_POINT ( 'NONE',  ( 0.000000000000000000, 5.541000000000003034, 3.956250000000000266 ) ) ;
#2658 = ORIENTED_EDGE ( 'NONE', *, *, #3526, .T. ) ;
#2659 = DIRECTION ( 'NONE',  ( 0.000000000000000000, 0.000000000000000000, 1.000000000000000000 ) ) ;
#2660 = DIRECTION ( 'NONE',  ( -1.000000000000000000, 0.000000000000000000, 0.000000000000000000 ) ) ;
#2661 = CARTESIAN_POINT ( 'NONE',  ( -3.987046614173228587, 3.757861515926525176, 8.272475195628263833 ) ) ;
#2662 = ORIENTED_EDGE ( 'NONE', *, *, #5198, .T. ) ;
#2663 = CARTESIAN_POINT ( 'NONE',  ( -8.751021560936518753E-10, 1.365923996832131609E-16, 3.874999999600099443 ) ) ;
#2664 = VERTEX_POINT ( 'NONE', #2700 ) ;
#2665 = CARTESIAN_POINT ( 'NONE',  ( -1.187499999999999778, 4.446597588353633057, 6.517308014370972735 ) ) ;
#2666 = COORDINATED_UNIVERSAL_TIME_OFFSET ( 0, 0, .AHEAD. ) ;
#2667 = ORIENTED_EDGE ( 'NONE', *, *, #7320, .T. ) ;
#2668 = SECURITY_CLASSIFICATION ( '', '', #4231 ) ;
#2669 = CC_DESIGN_DATE_AND_TIME_ASSIGNMENT ( #4421, #1351, ( #7597 ) ) ;
#2670 = CARTESIAN_POINT ( 'NONE',  ( 4.462953385826772923, 4.146499994075099060, 8.624249954778562710 ) ) ;
#2671 = CARTESIAN_POINT ( 'NONE',  ( -2.750000000000000888, 8.589000000000000412, 3.243476614173229411 ) ) ;
#2672 = PRODUCT_DEFINITION_SHAPE ( 'NONE', 'NONE',  #4922 ) ;
#2673 = CIRCLE ( 'NONE', #28, 0.3124999879509117728 ) ;
#2674 = CARTESIAN_POINT ( 'NONE',  ( 2.349999998660270872, 3.550000000000001155, -0.3883559095726498156 ) ) ;
#2675 = EDGE_CURVE ( 'NONE', #2861, #586, #7083, .T. ) ;
#2676 = ORIENTED_EDGE ( 'NONE', *, *, #5272, .F. ) ;
#2677 = DIRECTION ( 'NONE',  ( -1.000000000000000000, 0.000000000000000000, -0.000000000000000000 ) ) ;
#2678 = VERTEX_POINT ( 'NONE', #2118 ) ;
#2679 = AXIS2_PLACEMENT_3D ( 'NONE', #6401, #6441, #6932 ) ;
#2680 = VECTOR ( 'NONE', #2391, 39.37007874015748143 ) ;
#2681 = LINE ( 'NONE', #7666, #4752 ) ;
#2682 = CARTESIAN_POINT ( 'NONE',  ( 1.074999999999999289, 3.950000000000000178, 3.440250000000000696 ) ) ;
#2683 = AXIS2_PLACEMENT_3D ( 'NONE', #2824, #1602, #5229 ) ;
#2684 = EDGE_CURVE ( 'NONE', #4928, #3352, #4611, .T. ) ;
#2685 = CARTESIAN_POINT ( 'NONE',  ( 3.987953385826772390, 4.046209851940893110, 8.402619588493392300 ) ) ;
#2686 = EDGE_CURVE ( 'NONE', #2392, #1952, #6018, .T. ) ;
#2687 = ADVANCED_FACE ( 'NONE', ( #6011 ), #2927, .F. ) ;
#2688 = VERTEX_POINT ( 'NONE', #1094 ) ;
#2689 = EDGE_CURVE ( 'NONE', #5429, #3365, #2276, .T. ) ;
#2690 = AXIS2_PLACEMENT_3D ( 'NONE', #6302, #5635, #7042 ) ;
#2691 = VECTOR ( 'NONE', #6947, 39.37007874015748854 ) ;
#2692 = LINE ( 'NONE', #5176, #1389 ) ;
#2693 = PLANE ( 'NONE',  #850 ) ;
#2694 = ORIENTED_EDGE ( 'NONE', *, *, #4224, .F. ) ;
#2695 = ADVANCED_FACE ( 'NONE', ( #4192 ), #6676, .T. ) ;
#2696 = COORDINATED_UNIVERSAL_TIME_OFFSET ( 0, 0, .AHEAD. ) ;
#2697 = CARTESIAN_POINT ( 'NONE',  ( -2.745000000000000995, 7.973999999999999311, 3.828750000000002096 ) ) ;
#2698 = LINE ( 'NONE', #189, #560 ) ;
#2699 = CARTESIAN_POINT ( 'NONE',  ( 0.7274884641267199692, 4.132581358865608401, 8.485068404623115512 ) ) ;
#2700 = CARTESIAN_POINT ( 'NONE',  ( 3.987953385826772390, 3.950000015938371689, 8.543749986456024459 ) ) ;
#2701 = MANIFOLD_SOLID_BREP ( 'Imported1', #6743 ) ;
#2702 = EDGE_LOOP ( 'NONE', ( #4699, #6897, #1418, #4847, #2942 ) ) ;
#2703 = CARTESIAN_POINT ( 'NONE',  ( -3.987046614173227699, 4.132117433205395152, 8.157439729585876265 ) ) ;
#2704 = AXIS2_PLACEMENT_3D ( 'NONE', #2641, #1373, #124 ) ;
#2705 = CARTESIAN_POINT ( 'NONE',  ( -3.987046614173228587, 3.776897850682283231, 8.324661573291654904 ) ) ;
#2706 = VERTEX_POINT ( 'NONE', #4817 ) ;
#2707 = CARTESIAN_POINT ( 'NONE',  ( -2.150000000000000799, 5.025000000000000355, 3.440250000000000696 ) ) ;
#2708 = CARTESIAN_POINT ( 'NONE',  ( -2.750000000000000444, 8.574153543307087233, 4.323749999999999538 ) ) ;
#2709 = CARTESIAN_POINT ( 'NONE',  ( -2.750000000000000888, 7.964000000000000412, 3.333750000000001990 ) ) ;
#2710 = CALENDAR_DATE ( 2026, 8, 10 ) ;
#2711 = VERTEX_POINT ( 'NONE', #6708 ) ;
#2712 = CARTESIAN_POINT ( 'NONE',  ( -1.168432152159266657, 3.351763300421212399, -5.108749999999997904 ) ) ;
#2713 = CARTESIAN_POINT ( 'NONE',  ( 2.375000000000004441, 5.137500000000002842, 6.956249999999992717 ) ) ;
#2714 = VECTOR ( 'NONE', #5765, 39.37007874015748143 ) ;
#2715 = CARTESIAN_POINT ( 'NONE',  ( -1.201750196850394081, 2.500000000000000444, -0.5625000000000003331 ) ) ;
#2716 = APPROVAL_STATUS ( 'not_yet_approved' ) ;
#2717 = ORIENTED_EDGE ( 'NONE', *, *, #3419, .F. ) ;
#2718 = CARTESIAN_POINT ( 'NONE',  ( -3.296097360993826886, 2.500000000000000444, 0.5625000000000001110 ) ) ;
#2719 = CARTESIAN_POINT ( 'NONE',  ( 3.987953385826772834, 3.759071817854598763, 8.184594090536538857 ) ) ;
#2720 = CARTESIAN_POINT ( 'NONE',  ( 4.067120052493439886, 3.516000035344542862, 8.231249998505111520 ) ) ;
#2721 = CC_DESIGN_PERSON_AND_ORGANIZATION_ASSIGNMENT ( #443, #7907, ( #1622 ) ) ;
#2722 = CARTESIAN_POINT ( 'NONE',  ( 3.987953385826772834, 4.106701403461291200, 8.349863190999146312 ) ) ;
#2723 = ORIENTED_EDGE ( 'NONE', *, *, #1694, .T. ) ;
#2724 = EDGE_CURVE ( 'NONE', #5647, #586, #7162, .T. ) ;
#2725 = EDGE_CURVE ( 'NONE', #2302, #7663, #6833, .T. ) ;
#2726 = CARTESIAN_POINT ( 'NONE',  ( 0.000000000000000000, 2.499999999857933197, 0.000000000000000000 ) ) ;
#2727 = CARTESIAN_POINT ( 'NONE',  ( -1.172489672300577768, 1.000000000000000888, -3.693357952253316423 ) ) ;
#2728 = ORIENTED_EDGE ( 'NONE', *, *, #5371, .F. ) ;
#2729 = CALENDAR_DATE ( 2026, 8, 10 ) ;
#2730 = APPLICATION_CONTEXT ( 'configuration controlled 3d designs of mechanical parts and assemblies' ) ;
#2731 = EDGE_CURVE ( 'NONE', #6240, #1632, #4136, .T. ) ;
#2732 = DIRECTION ( 'NONE',  ( -1.000000000000000000, 0.000000000000000000, 0.000000000000000000 ) ) ;
#2733 = ITEM_DEFINED_TRANSFORMATION ( 'NONE', 'NONE', #7560,  #7272 ) ;
#2734 = PLANE ( 'NONE',  #964 ) ;
#2735 = CARTESIAN_POINT ( 'NONE',  ( 3.562500000000000444, -3.820994442221351629E-18, 3.337500000000003020 ) ) ;
#2736 = ORIENTED_EDGE ( 'NONE', *, *, #6294, .F. ) ;
#2737 = DIRECTION ( 'NONE',  ( -0.000000000000000000, -0.000000000000000000, 1.000000000000000000 ) ) ;
#2738 = CARTESIAN_POINT ( 'NONE',  ( -3.987046614173229475, 3.820636894295539321, 8.379777743323508332 ) ) ;
#2739 = ORIENTED_EDGE ( 'NONE', *, *, #3582, .T. ) ;
#2740 = CARTESIAN_POINT ( 'NONE',  ( 3.296097360985625002, 2.500000000000000444, -0.5625000000000001110 ) ) ;
#2741 = CYLINDRICAL_SURFACE ( 'NONE', #4118, 2.845000000000001528 ) ;
#2742 = PLANE ( 'NONE',  #1771 ) ;
#2743 = CARTESIAN_POINT ( 'NONE',  ( 1.625000000000000222, 3.950000000000000178, 2.750000000234376074 ) ) ;
#2744 = COORDINATED_UNIVERSAL_TIME_OFFSET ( 0, 0, .AHEAD. ) ;
#2745 = ORIENTED_EDGE ( 'NONE', *, *, #3499, .F. ) ;
#2746 = EDGE_CURVE ( 'NONE', #4873, #2544, #1304, .T. ) ;
#2747 = CARTESIAN_POINT ( 'NONE',  ( -1.261644052163539920, 4.312451747426980120, -5.108749999999998792 ) ) ;
#2748 = DIRECTION ( 'NONE',  ( -1.000000000000000000, 0.000000000000000000, -0.000000000000000000 ) ) ;
#2749 = CARTESIAN_POINT ( 'NONE',  ( 2.750000000000000444, 7.339000000000003077, 2.411250000000000338 ) ) ;
#2750 = PLANE ( 'NONE',  #3195 ) ;
#2751 = ORIENTED_EDGE ( 'NONE', *, *, #2309, .F. ) ;
#2752 = DATE_AND_TIME ( #1610, #5802 ) ;
#2753 = ORGANIZATION ( 'NAUO-ORG2', 'UNSPECIFIED', 'UNSPECIFIED' ) ;
#2754 = ORIENTED_EDGE ( 'NONE', *, *, #8148, .T. ) ;
#2755 = CARTESIAN_POINT ( 'NONE',  ( 0.000000000000000000, 1.664000000000000368, 2.693920355039552791E-42 ) ) ;
#2756 = DESIGN_CONTEXT ( 'detailed design', #1108, 'design' ) ;
#2757 = ORIENTED_EDGE ( 'NONE', *, *, #7788, .F. ) ;
#2758 = DIRECTION ( 'NONE',  ( -0.000000000000000000, -1.000000000000000000, -0.000000000000000000 ) ) ;
#2759 = DIRECTION ( 'NONE',  ( 0.000000000000000000, 0.000000000000000000, -1.000000000000000000 ) ) ;
#2760 = CARTESIAN_POINT ( 'NONE',  ( 2.740000000000001545, 7.964000000000000412, 3.833750000000001545 ) ) ;
#2761 = ORIENTED_EDGE ( 'NONE', *, *, #1733, .F. ) ;
#2762 = CC_DESIGN_PERSON_AND_ORGANIZATION_ASSIGNMENT ( #8154, #8112, ( #5941 ) ) ;
#2763 = CARTESIAN_POINT ( 'NONE',  ( 0.000000000000000000, 2.359000000000000874, 3.956250000000000266 ) ) ;
#2764 = CARTESIAN_POINT ( 'NONE',  ( 1.187500000000000444, 5.969165905511811587, 4.238473622047244760 ) ) ;
#2765 = EDGE_LOOP ( 'NONE', ( #2025, #5933 ) ) ;
#2766 = APPROVAL_ROLE ( '' ) ;
#2767 = LINE ( 'NONE', #5252, #7568 ) ;
#2768 = EDGE_CURVE ( 'NONE', #4783, #2678, #8002, .T. ) ;
#2769 = CONTEXT_DEPENDENT_SHAPE_REPRESENTATION ( #1940, #2604 ) ;
#2770 = DIRECTION ( 'NONE',  ( 1.000000000000000000, 0.000000000000000000, 0.000000000000000000 ) ) ;
#2771 = CARTESIAN_POINT ( 'NONE',  ( 1.312500000123273169, 7.352492868468935683, 3.316250000424603606 ) ) ;
#2772 = VERTEX_POINT ( 'NONE', #7523 ) ;
#2773 = DIRECTION ( 'NONE',  ( 0.000000000000000000, 0.000000000000000000, -1.000000000000000000 ) ) ;
#2774 = CARTESIAN_POINT ( 'NONE',  ( -3.987046614173230363, 4.098527760755414917, 8.360613120148601141 ) ) ;
#2775 = ORIENTED_EDGE ( 'NONE', *, *, #4013, .F. ) ;
#2776 = CARTESIAN_POINT ( 'NONE',  ( 0.000000000000000000, 1.750000000000000444, -2.845000000000001528 ) ) ;
#2777 = DIRECTION ( 'NONE',  ( 0.0005594472316432144016, -6.949735925632083422E-17, 0.9999998435093853111 ) ) ;
#2778 = CARTESIAN_POINT ( 'NONE',  ( -8.751021560936518753E-10, 1.365923996832131609E-16, 5.750408897959578548E-10 ) ) ;
#2779 = APPROVAL_STATUS ( 'not_yet_approved' ) ;
#2780 = SHAPE_REPRESENTATION ( 'bench vise9-', ( #7272 ), #1380 ) ;
#2781 = ORIENTED_EDGE ( 'NONE', *, *, #6281, .T. ) ;
#2782 = EDGE_CURVE ( 'NONE', #2992, #3502, #4370, .T. ) ;
#2783 = LINE ( 'NONE', #5270, #7537 ) ;
#2784 = EDGE_CURVE ( 'NONE', #3627, #3267, #3731, .T. ) ;
#2785 = CARTESIAN_POINT ( 'NONE',  ( -0.6955818286634507519, 2.836155590436416851, -5.108750000000003233 ) ) ;
#2786 = CARTESIAN_POINT ( 'NONE',  ( -0.7631207261360639649, 5.018067241527451650, -5.108749999999999680 ) ) ;
#2787 = CARTESIAN_POINT ( 'NONE',  ( -2.750000000000000444, 7.964000000000000412, 4.323750000000003091 ) ) ;
#2788 = CARTESIAN_POINT ( 'NONE',  ( 2.750000000000000888, 8.574153543307089009, 3.323750000000001315 ) ) ;
#2789 =( NAMED_UNIT ( * ) PLANE_ANGLE_UNIT ( ) SI_UNIT ( $, .RADIAN. ) );
#2790 = ORIENTED_EDGE ( 'NONE', *, *, #5629, .F. ) ;
#2791 = DATE_TIME_ROLE ( 'classification_date' ) ;
#2792 = EDGE_CURVE ( 'NONE', #6928, #987, #2194, .T. ) ;
#2793 = ORIENTED_EDGE ( 'NONE', *, *, #7314, .T. ) ;
#2794 = AXIS2_PLACEMENT_3D ( 'NONE', #7179, #5821, #5317 ) ;
#2795 = DIRECTION ( 'NONE',  ( 0.000000000000000000, 0.000000000000000000, 1.000000000000000000 ) ) ;
#2796 = LOCAL_TIME ( 0, 37, 23.00000000000000000, #3714 ) ;
#2797 = AXIS2_PLACEMENT_3D ( 'NONE', #6283, #6780, #3664 ) ;
#2798 = PRODUCT_DEFINITION_FORMATION_WITH_SPECIFIED_SOURCE ( 'ANY', '', #1432, .NOT_KNOWN. ) ;
#2799 = CARTESIAN_POINT ( 'NONE',  ( 1.054418147088230118, 4.854198014699673713, 6.858307716535437137 ) ) ;
#2800 = LINE ( 'NONE', #7753, #6725 ) ;
#2801 = PLANE ( 'NONE',  #2445 ) ;
#2802 = LOCAL_TIME ( 0, 37, 23.00000000000000000, #234 ) ;
#2803 = ADVANCED_FACE ( 'NONE', ( #1431 ), #1958, .F. ) ;
#2804 = CARTESIAN_POINT ( 'NONE',  ( 3.987953385826772390, 4.037524053344319519, 8.407402232862313696 ) ) ;
#2805 = ORIENTED_EDGE ( 'NONE', *, *, #6398, .T. ) ;
#2806 = VECTOR ( 'NONE', #2220, 39.37007874015748143 ) ;
#2807 = EDGE_CURVE ( 'NONE', #2981, #1998, #1803, .T. ) ;
#2808 = VECTOR ( 'NONE', #5571, 39.37007874015748143 ) ;
#2809 = CARTESIAN_POINT ( 'NONE',  ( 1.500000000000000444, 5.639000000000001123, 0.5414159055118110686 ) ) ;
#2810 = AXIS2_PLACEMENT_3D ( 'NONE', #552, #2330, #3052 ) ;
#2811 =( GEOMETRIC_REPRESENTATION_CONTEXT ( 3 ) GLOBAL_UNCERTAINTY_ASSIGNED_CONTEXT ( ( #3889 ) ) GLOBAL_UNIT_ASSIGNED_CONTEXT ( ( #908, #2789, #7225 ) ) REPRESENTATION_CONTEXT ( 'NONE', 'WORKASPACE' ) );
#2812 = CARTESIAN_POINT ( 'NONE',  ( 2.740000000000000213, 8.729000000000002757, 3.813750000000002416 ) ) ;
#2813 = COORDINATED_UNIVERSAL_TIME_OFFSET ( 0, 0, .AHEAD. ) ;
#2814 = DIRECTION ( 'NONE',  ( -0.000000000000000000, -0.000000000000000000, 1.000000000000000000 ) ) ;
#2815 = CC_DESIGN_DATE_AND_TIME_ASSIGNMENT ( #3681, #2941, ( #1832 ) ) ;
#2816 = CARTESIAN_POINT ( 'NONE',  ( 0.7499999999999995559, 3.970887754116599666, 7.918750000000000178 ) ) ;
#2817 = CLOSED_SHELL ( 'NONE', ( #5342, #129, #425, #7525, #5808, #6795, #61, #1834, #6900, #6277, #7109, #5405, #1979, #6758, #5478, #6981, #4530, #5582, #5119, #5125, #1226, #2277, #1092, #2978, #6252, #276, #2143, #5839, #1332, #5921, #6605, #6253, #2830, #6323, #7573, #4427, #5737 ) ) ;
#2818 = ORIENTED_EDGE ( 'NONE', *, *, #2542, .T. ) ;
#2819 = CARTESIAN_POINT ( 'NONE',  ( -3.182000000000000828, 5.541000000000003922, 3.956250000000000266 ) ) ;
#2820 = LINE ( 'NONE', #7865, #7116 ) ;
#2821 = ORIENTED_EDGE ( 'NONE', *, *, #3137, .F. ) ;
#2822 = LINE ( 'NONE', #1557, #1512 ) ;
#2823 = EDGE_LOOP ( 'NONE', ( #5080, #5628, #4023, #770, #696, #628 ) ) ;
#2824 = CARTESIAN_POINT ( 'NONE',  ( 0.000000000000000000, 2.500000000130568889, 0.000000000000000000 ) ) ;
#2825 = CALENDAR_DATE ( 2026, 8, 10 ) ;
#2826 = VERTEX_POINT ( 'NONE', #59 ) ;
#2827 = AXIS2_PLACEMENT_3D ( 'NONE', #1016, #6009, #2274 ) ;
#2828 = CARTESIAN_POINT ( 'NONE',  ( -1.116010548110457856, 3.257898045036971002, -5.108750000000001457 ) ) ;
#2829 = FACE_OUTER_BOUND ( 'NONE', #6089, .T. ) ;
#2830 = ADVANCED_FACE ( 'NONE', ( #2576, #7606 ), #12, .T. ) ;
#2831 =( BOUNDED_SURFACE ( )  B_SPLINE_SURFACE ( 3, 3, ( 
 ( #723, #3217, #6379, #1298 ),
 ( #4525, #3822, #3788, #5596 ),
 ( #7039, #5722, #2607, #603 ),
 ( #1258, #1422, #4441, #5674 ) ),
 .UNSPECIFIED., .F., .F., .F. ) 
 B_SPLINE_SURFACE_WITH_KNOTS ( ( 4, 4 ),
 ( 4, 4 ),
 ( 0.000000000000000000, 1.000000000000000000 ),
 ( 0.000000000000000000, 1.000000000000000000 ),
 .UNSPECIFIED. ) 
 GEOMETRIC_REPRESENTATION_ITEM ( )  RATIONAL_B_SPLINE_SURFACE ( (
 ( 1.000000000000000000, 0.3333333333333330373, 0.3333333333333330373, 1.000000000000000000),
 ( 0.8047378541243660477, 0.2682459513747890156, 0.2682459513747890156, 0.8047378541243660477),
 ( 0.8047378541243660477, 0.2682459513747890156, 0.2682459513747890156, 0.8047378541243660477),
 ( 1.000000000000000000, 0.3333333333333330373, 0.3333333333333330373, 1.000000000000000000) ) ) 
 REPRESENTATION_ITEM ( '' )  SURFACE ( )  );
#2832 = CARTESIAN_POINT ( 'NONE',  ( 1.624999999905518688, 3.950000000000000178, 2.749999999885571533 ) ) ;
#2833 = AXIS2_PLACEMENT_3D ( 'NONE', #5223, #7769, #734 ) ;
#2834 = PERSON_AND_ORGANIZATION_ROLE ( 'creator' ) ;
#2835 = ORIENTED_EDGE ( 'NONE', *, *, #3251, .T. ) ;
#2836 = EDGE_CURVE ( 'NONE', #4873, #6966, #3112, .T. ) ;
#2837 = CARTESIAN_POINT ( 'NONE',  ( 2.750000000000000444, 7.973999999999999311, 3.833750000000001545 ) ) ;
#2838 = VECTOR ( 'NONE', #1903, 39.37007874015748143 ) ;
#2839 = AXIS2_PLACEMENT_3D ( 'NONE', #4195, #7386, #3786 ) ;
#2840 = AXIS2_PLACEMENT_3D ( 'NONE', #2718, #5206, #2677 ) ;
#2841 = DIRECTION ( 'NONE',  ( 0.000000000000000000, 0.000000000000000000, 1.000000000000000000 ) ) ;
#2842 = CARTESIAN_POINT ( 'NONE',  ( -3.343750000000001776, 1.750000000000000444, 0.5625000000000003331 ) ) ;
#2843 = ORIENTED_EDGE ( 'NONE', *, *, #6709, .T. ) ;
#2844 = CARTESIAN_POINT ( 'NONE',  ( -0.7335700382782335272, 2.500000000365355302, -5.108750000000001457 ) ) ;
#2845 = ORIENTED_EDGE ( 'NONE', *, *, #7928, .T. ) ;
#2846 = CARTESIAN_POINT ( 'NONE',  ( -3.987046614173229475, 4.140928214022093989, 8.184594090536863931 ) ) ;
#2847 = PLANE ( 'NONE',  #5179 ) ;
#2848 = CYLINDRICAL_SURFACE ( 'NONE', #6488, 3.874999999025058539 ) ;
#2849 = ORIENTED_EDGE ( 'NONE', *, *, #6036, .T. ) ;
#2850 = COORDINATED_UNIVERSAL_TIME_OFFSET ( 0, 0, .AHEAD. ) ;
#2851 = LINE ( 'NONE', #3512, #1243 ) ;
#2852 = COORDINATED_UNIVERSAL_TIME_OFFSET ( 0, 0, .AHEAD. ) ;
#2853 = CARTESIAN_POINT ( 'NONE',  ( 0.6994518761186668820, 4.220944655642501431, 8.074232055893794779 ) ) ;
#2854 = FACE_OUTER_BOUND ( 'NONE', #7085, .T. ) ;
#2855 = CC_DESIGN_APPROVAL ( #5165, ( #2206 ) ) ;
#2856 = EDGE_LOOP ( 'NONE', ( #54, #4216, #5574, #2170, #4541 ) ) ;
#2857 = CARTESIAN_POINT ( 'NONE',  ( 0.000000000000000000, 5.376007322834645663, 5.972081456692916568 ) ) ;
#2858 = PLANE ( 'NONE',  #1246 ) ;
#2859 = CARTESIAN_POINT ( 'NONE',  ( -2.750000000000000444, 8.719000000000001194, 3.333750000000001990 ) ) ;
#2860 = CARTESIAN_POINT ( 'NONE',  ( 2.750000000000000888, 8.719000000000001194, 3.333750000000001990 ) ) ;
#2861 = VERTEX_POINT ( 'NONE', #1992 ) ;
#2862 = CALENDAR_DATE ( 2026, 8, 10 ) ;
#2863 = FACE_OUTER_BOUND ( 'NONE', #4049, .T. ) ;
#2864 = COORDINATED_UNIVERSAL_TIME_OFFSET ( 0, 0, .AHEAD. ) ;
#2865 = EDGE_CURVE ( 'NONE', #822, #4281, #6305, .T. ) ;
#2866 = ORIENTED_EDGE ( 'NONE', *, *, #239, .T. ) ;
#2867 = DIRECTION ( 'NONE',  ( -1.000000000000000000, -0.000000000000000000, 0.000000000000000000 ) ) ;
#2868 = CARTESIAN_POINT ( 'NONE',  ( -0.2166615117570589999, 2.654796885154087516, -5.108749999999997904 ) ) ;
#2869 = LINE ( 'NONE', #5357, #3628 ) ;
#2870 = CC_DESIGN_PERSON_AND_ORGANIZATION_ASSIGNMENT ( #4207, #4130, ( #1319 ) ) ;
#2871 = LINE ( 'NONE', #863, #3591 ) ;
#2872 = CARTESIAN_POINT ( 'NONE',  ( -1.312500000000000444, 7.352492870354978116, 3.316250000370397188 ) ) ;
#2873 = APPROVAL_STATUS ( 'not_yet_approved' ) ;
#2874 = EDGE_LOOP ( 'NONE', ( #3303, #359, #8000, #3343 ) ) ;
#2875 = ADVANCED_FACE ( 'NONE', ( #3761 ), #3184, .F. ) ;
#2876 =( BOUNDED_SURFACE ( )  B_SPLINE_SURFACE ( 3, 3, ( 
 ( #483, #1797, #7387, #4288 ),
 ( #2412, #7944, #7994, #4781 ),
 ( #3641, #2282, #6139, #519 ),
 ( #1714, #3013, #1211, #2979 ),
 ( #7438, #5385, #6679, #1176 ),
 ( #3676, #440, #6755, #6791 ) ),
 .UNSPECIFIED., .F., .F., .F. ) 
 B_SPLINE_SURFACE_WITH_KNOTS ( ( 4, 2, 4 ),
 ( 4, 4 ),
 ( 0.000000000000000000, 0.5000000000000000000, 1.000000000000000000 ),
 ( 0.000000000000000000, 1.000000000000000000 ),
 .UNSPECIFIED. ) 
 GEOMETRIC_REPRESENTATION_ITEM ( )  RATIONAL_B_SPLINE_SURFACE ( (
 ( 1.000000000000000000, 0.3333333333333334259, 0.3333333333333334259, 1.000000000000000000),
 ( 1.000000000000000000, 0.3333333333333334259, 0.3333333333333334259, 1.000000000000000000),
 ( 1.000000000000000000, 0.3333333333333334259, 0.3333333333333334259, 1.000000000000000000),
 ( 1.000000000000000000, 0.3333333333333334259, 0.3333333333333334259, 1.000000000000000000),
 ( 1.000000000000000000, 0.3333333333333334259, 0.3333333333333334259, 1.000000000000000000),
 ( 1.000000000000000000, 0.3333333333333334259, 0.3333333333333334259, 1.000000000000000000) ) ) 
 REPRESENTATION_ITEM ( '' )  SURFACE ( )  );
#2877 = EDGE_CURVE ( 'NONE', #938, #4460, #767, .T. ) ;
#2878 = CARTESIAN_POINT ( 'NONE',  ( -2.537500000000000533, 2.500000000000000444, -0.2625000000000008438 ) ) ;
#2879 = LINE ( 'NONE', #7282, #3186 ) ;
#2880 = DIRECTION ( 'NONE',  ( -1.000000000000000000, 0.000000000000000000, 0.000000000000000000 ) ) ;
#2881 = EDGE_LOOP ( 'NONE', ( #708, #7493, #6007, #2989 ) ) ;
#2882 = EDGE_CURVE ( 'NONE', #4311, #520, #5766, .T. ) ;
#2883 = CARTESIAN_POINT ( 'NONE',  ( -3.987046614173226811, 3.876126805297171796, 8.049163100252911818 ) ) ;
#2884 = FACE_OUTER_BOUND ( 'NONE', #3624, .T. ) ;
#2885 = DIRECTION ( 'NONE',  ( -0.5773502691896257311, 0.5773502691896257311, 0.5773502691896257311 ) ) ;
#2886 = PERSON_AND_ORGANIZATION_ROLE ( 'creator' ) ;
#2887 = DIRECTION ( 'NONE',  ( 0.000000000000000000, 0.000000000000000000, 1.000000000000000000 ) ) ;
#2888 = CALENDAR_DATE ( 2026, 8, 10 ) ;
#2889 = CARTESIAN_POINT ( 'NONE',  ( 0.7210596466522595227, 4.156871429633926418, 7.996158673814920625 ) ) ;
#2890 = ORIENTED_EDGE ( 'NONE', *, *, #3027, .T. ) ;
#2891 = DIRECTION ( 'NONE',  ( 0.000000000000000000, 0.000000000000000000, -1.000000000000000000 ) ) ;
#2892 = DIRECTION ( 'NONE',  ( 0.000000000000000000, -1.000000000000000000, 0.000000000000000000 ) ) ;
#2893 = DIRECTION ( 'NONE',  ( 0.1278538907425633420, 0.000000000000000000, -0.9917930140014037388 ) ) ;
#2894 = CARTESIAN_POINT ( 'NONE',  ( -2.875000000000000888, 1.000000000000000222, -2.975000000000000977 ) ) ;
#2895 = ORIENTED_EDGE ( 'NONE', *, *, #7186, .F. ) ;
#2896 = DIRECTION ( 'NONE',  ( -0.000000000000000000, 0.000000000000000000, -1.000000000000000000 ) ) ;
#2897 = CALENDAR_DATE ( 2026, 8, 10 ) ;
#2898 = EDGE_CURVE ( 'NONE', #5232, #6380, #3503, .T. ) ;
#2899 = ORIENTED_EDGE ( 'NONE', *, *, #7153, .T. ) ;
#2900 = FACE_OUTER_BOUND ( 'NONE', #6016, .T. ) ;
#2901 = CARTESIAN_POINT ( 'NONE',  ( 0.000000000000000000, 3.950000000000000178, 3.691250000234376216 ) ) ;
#2902 = CARTESIAN_POINT ( 'NONE',  ( -3.687499989627468722, 1.365923996832131609E-16, 3.874999999790589289 ) ) ;
#2903 = CARTESIAN_POINT ( 'NONE',  ( -2.875000000000000888, 1.000000000000000222, -3.337500001222715174 ) ) ;
#2904 = LINE ( 'NONE', #3492, #1233 ) ;
#2905 = COORDINATED_UNIVERSAL_TIME_OFFSET ( 0, 0, .AHEAD. ) ;
#2906 = EDGE_LOOP ( 'NONE', ( #3129, #6923, #2327, #6570 ) ) ;
#2907 = CARTESIAN_POINT ( 'NONE',  ( -4.462046614173229564, 4.146499994074616779, 8.231249998505111520 ) ) ;
#2908 = APPROVAL ( #2779, 'UNSPECIFIED' ) ;
#2909 = DESIGN_CONTEXT ( 'detailed design', #4294, 'design' ) ;
#2910 = CARTESIAN_POINT ( 'NONE',  ( -8.751021560936518753E-10, 1.000000000000000222, 5.750408897959578548E-10 ) ) ;
#2911 = VECTOR ( 'NONE', #6386, 39.37007874015748143 ) ;
#2912 = LINE ( 'NONE', #8056, #701 ) ;
#2913 = CARTESIAN_POINT ( 'NONE',  ( -2.861675873811764248, 1.000000000000000222, -2.612744953730403719 ) ) ;
#2914 = CARTESIAN_POINT ( 'NONE',  ( -2.750000000000000888, 7.974000000000001087, 3.813750000000002416 ) ) ;
#2915 = ORIENTED_EDGE ( 'NONE', *, *, #1322, .T. ) ;
#2916 = LOCAL_TIME ( 0, 37, 23.00000000000000000, #2185 ) ;
#2917 = EDGE_CURVE ( 'NONE', #1059, #2209, #4331, .T. ) ;
#2918 = CARTESIAN_POINT ( 'NONE',  ( -3.987046614173228587, 4.128161578177576452, 8.148241431726020778 ) ) ;
#2919 = DIRECTION ( 'NONE',  ( 0.000000000000000000, -1.000000000000000000, 0.000000000000000000 ) ) ;
#2920 = EDGE_CURVE ( 'NONE', #6239, #584, #4100, .T. ) ;
#2921 = DIRECTION ( 'NONE',  ( 0.000000000000000000, 1.000000000000000000, 0.000000000000000000 ) ) ;
#2922 = ORIENTED_EDGE ( 'NONE', *, *, #6989, .T. ) ;
#2923 = PERSON_AND_ORGANIZATION ( #7862, #8117 ) ;
#2924 = VECTOR ( 'NONE', #5452, 39.37007874015748143 ) ;
#2925 = DIRECTION ( 'NONE',  ( -0.000000000000000000, -1.000000000000000000, -0.000000000000000000 ) ) ;
#2926 = APPLICATION_CONTEXT ( 'configuration controlled 3d designs of mechanical parts and assemblies' ) ;
#2927 = PLANE ( 'NONE',  #2577 ) ;
#2928 = EDGE_CURVE ( 'NONE', #1007, #5688, #4910, .T. ) ;
#2929 = AXIS2_PLACEMENT_3D ( 'NONE', #1529, #6067, #4744 ) ;
#2930 = CIRCLE ( 'NONE', #2148, 3.874999999025058539 ) ;
#2931 = ORIENTED_EDGE ( 'NONE', *, *, #7197, .T. ) ;
#2932 = CC_DESIGN_SECURITY_CLASSIFICATION ( #1242, ( #8193 ) ) ;
#2933 = EDGE_CURVE ( 'NONE', #843, #7238, #3427, .T. ) ;
#2934 = FACE_OUTER_BOUND ( 'NONE', #319, .T. ) ;
#2935 = ORIENTED_EDGE ( 'NONE', *, *, #177, .F. ) ;
#2936 = CARTESIAN_POINT ( 'NONE',  ( 2.537499998660271761, 3.550000000000001155, 0.3883559095726499266 ) ) ;
#2937 = ORIENTED_EDGE ( 'NONE', *, *, #5242, .F. ) ;
#2938 = PERSON_AND_ORGANIZATION_ROLE ( 'creator' ) ;
#2939 = PLANE ( 'NONE',  #7006 ) ;
#2940 = AXIS2_PLACEMENT_3D ( 'NONE', #3715, #1064, #8076 ) ;
#2941 = DATE_TIME_ROLE ( 'classification_date' ) ;
#2942 = ORIENTED_EDGE ( 'NONE', *, *, #5367, .F. ) ;
#2943 = VECTOR ( 'NONE', #7076, 39.37007874015748143 ) ;
#2944 = LINE ( 'NONE', #6106, #880 ) ;
#2945 = CC_DESIGN_APPROVAL ( #1614, ( #1579 ) ) ;
#2946 = LINE ( 'NONE', #1391, #3187 ) ;
#2947 = CARTESIAN_POINT ( 'NONE',  ( 0.03134105979970094186, 2.325218920766706887, 3.079992493227982298 ) ) ;
#2948 = AXIS2_PLACEMENT_3D ( 'NONE', #5132, #3787, #7678 ) ;
#2949 = APPROVAL_PERSON_ORGANIZATION ( #1826, #3264, #7227 ) ;
#2950 = CARTESIAN_POINT ( 'NONE',  ( -0.7188803599037373315, 4.163931010176847636, 8.003234414602300006 ) ) ;
#2951 =( LENGTH_UNIT ( ) NAMED_UNIT ( * ) SI_UNIT ( $, .METRE. ) );
#2952 = CARTESIAN_POINT ( 'NONE',  ( -2.875000000000000888, -3.820994292482255198E-18, -2.612499998777286780 ) ) ;
#2953 = SHAPE_DEFINITION_REPRESENTATION ( #7500, #4229 ) ;
#2954 = VERTEX_POINT ( 'NONE', #4533 ) ;
#2955 = CARTESIAN_POINT ( 'NONE',  ( 3.362499999999999822, 1.750000000000000222, -6.725000000000002309 ) ) ;
#2956 = CIRCLE ( 'NONE', #7839, 1.624999999999999778 ) ;
#2957 = FACE_OUTER_BOUND ( 'NONE', #7468, .T. ) ;
#2958 = AXIS2_PLACEMENT_3D ( 'NONE', #4114, #6641, #7863 ) ;
#2959 = CARTESIAN_POINT ( 'NONE',  ( 2.740000000000001545, 0.000000000000000000, 4.323750000000001315 ) ) ;
#2960 = CARTESIAN_POINT ( 'NONE',  ( -3.562500000000000444, 1.000000000000000222, 2.612499999999998934 ) ) ;
#2961 = ORIENTED_EDGE ( 'NONE', *, *, #6808, .T. ) ;
#2962 = DIRECTION ( 'NONE',  ( 1.000000000000000000, -0.000000000000000000, 2.606890220986081510E-17 ) ) ;
#2963 = ORIENTED_EDGE ( 'NONE', *, *, #3739, .F. ) ;
#2964 = VECTOR ( 'NONE', #892, 39.37007874015748143 ) ;
#2965 = LINE ( 'NONE', #2232, #7673 ) ;
#2966 = LINE ( 'NONE', #4226, #5930 ) ;
#2967 = PRODUCT_RELATED_PRODUCT_CATEGORY ( 'detail', '', ( #5212 ) ) ;
#2968 = LINE ( 'NONE', #2449, #7540 ) ;
#2969 = CARTESIAN_POINT ( 'NONE',  ( -3.544128229492827575, 1.000000000000000222, 1.972857802467875565 ) ) ;
#2970 = FACE_OUTER_BOUND ( 'NONE', #4556, .T. ) ;
#2971 = ORIENTED_EDGE ( 'NONE', *, *, #887, .T. ) ;
#2972 = AXIS2_PLACEMENT_3D ( 'NONE', #5831, #1570, #1534 ) ;
#2973 = PERSON_AND_ORGANIZATION ( #7862, #8117 ) ;
#2974 = DIRECTION ( 'NONE',  ( -1.000000000000000000, 0.000000000000000000, -0.000000000000000000 ) ) ;
#2975 =( BOUNDED_SURFACE ( )  B_SPLINE_SURFACE ( 2, 1, ( 
 ( #2788, #156 ),
 ( #5825, #2671 ),
 ( #1444, #2059 ),
 ( #3321, #208 ),
 ( #7746, #7099 ),
 ( #2749, #1481 ),
 ( #6491, #5236 ),
 ( #7831, #6029 ),
 ( #414, #1034 ),
 ( #5570, #1964 ),
 ( #2583, #7611 ) ),
 .UNSPECIFIED., .F., .F., .F. ) 
 B_SPLINE_SURFACE_WITH_KNOTS ( ( 3, 2, 2, 2, 2, 3 ),
 ( 2, 2 ),
 ( 1.337827206813319902, 1.570796326794899889, 3.141592653589790007, 4.712388980384690562, 5.497197239955569081, 5.538790940286991926 ),
 ( 0.000000000000000000, 1.000000000000000000 ),
 .UNSPECIFIED. ) 
 GEOMETRIC_REPRESENTATION_ITEM ( )  RATIONAL_B_SPLINE_SURFACE ( (
 ( 0.9260057553135151442, 0.9260057553135151442),
 ( 0.9565602018087399072, 0.9565602018087399072),
 ( 1.000000000000000000, 1.000000000000000000),
 ( 0.7071067811865479058, 0.7071067811865479058),
 ( 1.000000000000000000, 1.000000000000000000),
 ( 0.7071067811865479058, 0.7071067811865479058),
 ( 1.000000000000000000, 1.000000000000000000),
 ( 0.8536633850130519452, 0.8536633850130519452),
 ( 0.8535534732088591037, 0.8535534732088591037),
 ( 0.8535534732088591037, 0.8535534732088591037),
 ( 0.8535534732088591037, 0.8535534732088591037) ) ) 
 REPRESENTATION_ITEM ( '' )  SURFACE ( )  );
#2976 = ORIENTED_EDGE ( 'NONE', *, *, #1426, .T. ) ;
#2977 = CARTESIAN_POINT ( 'NONE',  ( 2.537499998660271761, 3.362500000000000711, -1.169467086614173645 ) ) ;
#2978 = ADVANCED_FACE ( 'NONE', ( #7043 ), #1552, .F. ) ;
#2979 = CARTESIAN_POINT ( 'NONE',  ( -4.066213280839896527, 3.516000035344541974, 8.231249998505111520 ) ) ;
#2980 = FACE_OUTER_BOUND ( 'NONE', #7220, .T. ) ;
#2981 = VERTEX_POINT ( 'NONE', #2612 ) ;
#2982 = DIRECTION ( 'NONE',  ( -0.000000000000000000, 1.000000000000000000, -0.000000000000000000 ) ) ;
#2983 = CARTESIAN_POINT ( 'NONE',  ( 1.274606805354365768, 2.434036455968486834, 2.749999999536767437 ) ) ;
#2984 = CARTESIAN_POINT ( 'NONE',  ( -1.187500000000000222, 4.987711023622046547, 4.083473622047245399 ) ) ;
#2985 = VERTEX_POINT ( 'NONE', #5889 ) ;
#2986 = CARTESIAN_POINT ( 'NONE',  ( -0.6994737761126073039, 4.220893194183548580, 8.074121781180345181 ) ) ;
#2987 = PLANE ( 'NONE',  #4908 ) ;
#2988 = PERSON_AND_ORGANIZATION ( #7862, #8117 ) ;
#2989 = ORIENTED_EDGE ( 'NONE', *, *, #4992, .T. ) ;
#2990 = CARTESIAN_POINT ( 'NONE',  ( 1.312500000061636696, 4.908106857212807483, 2.750000000234376074 ) ) ;
#2991 = EDGE_CURVE ( 'NONE', #2473, #417, #2698, .T. ) ;
#2992 = VERTEX_POINT ( 'NONE', #802 ) ;
#2993 = DIRECTION ( 'NONE',  ( -0.9925485533740562305, -0.000000000000000000, -0.1218497812680350845 ) ) ;
#2994 = FACE_OUTER_BOUND ( 'NONE', #8097, .T. ) ;
#2995 = ORIENTED_EDGE ( 'NONE', *, *, #5095, .F. ) ;
#2996 = DIRECTION ( 'NONE',  ( -0.7071067811865475727, 0.7071067811865475727, 0.000000000000000000 ) ) ;
#2997 = ORIENTED_EDGE ( 'NONE', *, *, #8040, .T. ) ;
#2998 = CARTESIAN_POINT ( 'NONE',  ( 3.343750000000001776, 2.500000000000000444, 2.909883779527559611 ) ) ;
#2999 = ADVANCED_FACE ( 'NONE', ( #5764, #4609 ), #2734, .T. ) ;
#3000 = CARTESIAN_POINT ( 'NONE',  ( -2.750000000000000888, 7.974000000000001087, 3.823750000000002647 ) ) ;
#3001 = PRODUCT_DEFINITION_SHAPE ( 'NONE', 'NONE',  #2483 ) ;
#3002 = DIRECTION ( 'NONE',  ( 0.000000000000000000, -1.000000000000000000, 0.000000000000000000 ) ) ;
#3003 = FACE_BOUND ( 'NONE', #7013, .T. ) ;
#3004 = VERTEX_POINT ( 'NONE', #6519 ) ;
#3005 = PERSON_AND_ORGANIZATION_ROLE ( 'creator' ) ;
#3006 = CARTESIAN_POINT ( 'NONE',  ( 3.362500000000001155, 1.750000000000000222, 6.725000000000002309 ) ) ;
#3007 = APPROVAL ( #2873, 'UNSPECIFIED' ) ;
#3008 = SECURITY_CLASSIFICATION ( '', '', #5298 ) ;
#3009 = ORIENTED_EDGE ( 'NONE', *, *, #3039, .F. ) ;
#3010 = CARTESIAN_POINT ( 'NONE',  ( -8.751021560936518753E-10, 1.365923996832131609E-16, 5.750408897959578548E-10 ) ) ;
#3011 = LOCAL_TIME ( 0, 37, 23.00000000000000000, #7961 ) ;
#3012 = ADVANCED_FACE ( 'NONE', ( #3869 ), #5219, .T. ) ;
#3013 = CARTESIAN_POINT ( 'NONE',  ( -4.066213280839894750, 4.383999996532201848, 7.363250037317452090 ) ) ;
#3014 = EDGE_LOOP ( 'NONE', ( #5768, #390, #2676 ) ) ;
#3015 = APPLICATION_PROTOCOL_DEFINITION ( 'international standard', 'config_control_design', 1994, #6135 ) ;
#3016 = DIRECTION ( 'NONE',  ( 0.000000000000000000, 0.000000000000000000, -1.000000000000000000 ) ) ;
#3017 = PERSON_AND_ORGANIZATION_ROLE ( 'classification_officer' ) ;
#3018 = CARTESIAN_POINT ( 'NONE',  ( 0.7335700383277801162, 2.500000000390421473, -2.908930215353081383 ) ) ;
#3019 = DIRECTION ( 'NONE',  ( 0.000000000000000000, -0.000000000000000000, 1.000000000000000000 ) ) ;
#3020 = EDGE_CURVE ( 'NONE', #3236, #3210, #7811, .T. ) ;
#3021 = ORIENTED_EDGE ( 'NONE', *, *, #5752, .T. ) ;
#3022 = CARTESIAN_POINT ( 'NONE',  ( -0.6889980206436411292, 4.246403994982890673, 8.332369961285714055 ) ) ;
#3023 = EDGE_CURVE ( 'NONE', #6365, #584, #6324, .T. ) ;
#3024 = PERSON_AND_ORGANIZATION ( #7862, #8117 ) ;
#3025 = EDGE_LOOP ( 'NONE', ( #1569, #4007, #636, #4563 ) ) ;
#3026 = CARTESIAN_POINT ( 'NONE',  ( 2.750000000000000444, 8.729000000000002757, 3.833750000000001545 ) ) ;
#3027 = EDGE_CURVE ( 'NONE', #5045, #1666, #109, .T. ) ;
#3028 = ORIENTED_EDGE ( 'NONE', *, *, #6740, .F. ) ;
#3029 = CARTESIAN_POINT ( 'NONE',  ( -4.470366334113919926, 1.000000000000000222, 2.937534001674282358 ) ) ;
#3030 = PLANE ( 'NONE',  #835 ) ;
#3031 = ADVANCED_FACE ( 'NONE', ( #7662 ), #7751, .T. ) ;
#3032 = LINE ( 'NONE', #1079, #5269 ) ;
#3033 = CARTESIAN_POINT ( 'NONE',  ( 1.312500000000000444, 5.969165905511811587, 0.5414159055118111796 ) ) ;
#3034 = VERTEX_POINT ( 'NONE', #377 ) ;
#3035 = ORIENTED_EDGE ( 'NONE', *, *, #4661, .T. ) ;
#3036 = APPROVAL_PERSON_ORGANIZATION ( #1337, #7084, #1833 ) ;
#3037 = CARTESIAN_POINT ( 'NONE',  ( 3.063407152847613446, 2.250083286476321831, -0.5624999999737114731 ) ) ;
#3038 = DIRECTION ( 'NONE',  ( 0.000000000000000000, 0.000000000000000000, 1.000000000000000000 ) ) ;
#3039 = EDGE_CURVE ( 'NONE', #3123, #4445, #419, .T. ) ;
#3040 = CARTESIAN_POINT ( 'NONE',  ( -1.465509921259843251, 2.890529173228346682, -7.381560866141734678 ) ) ;
#3041 = CARTESIAN_POINT ( 'NONE',  ( 2.187663376927555706E-18, 3.950000000000000178, 0.5414159055118110686 ) ) ;
#3042 = CARTESIAN_POINT ( 'NONE',  ( 2.861675873811764248, 1.000000000000000222, -2.612744953730403719 ) ) ;
#3043 = VERTEX_POINT ( 'NONE', #4798 ) ;
#3044 = DATE_TIME_ROLE ( 'classification_date' ) ;
#3045 = CARTESIAN_POINT ( 'NONE',  ( -8.751021560936518753E-10, 1.000000000000000222, 5.750408897959578548E-10 ) ) ;
#3046 = AXIS2_PLACEMENT_3D ( 'NONE', #4885, #6041, #6629 ) ;
#3047 = AXIS2_PLACEMENT_3D ( 'NONE', #2420, #3019, #6179 ) ;
#3048 = LOCAL_TIME ( 0, 37, 23.00000000000000000, #6822 ) ;
#3049 = VERTEX_POINT ( 'NONE', #7326 ) ;
#3050 = VECTOR ( 'NONE', #7430, 39.37007874015748143 ) ;
#3051 = PLANE ( 'NONE',  #221 ) ;
#3052 = DIRECTION ( 'NONE',  ( 1.000000000000000000, 0.000000000000000000, -0.000000000000000000 ) ) ;
#3053 = DIRECTION ( 'NONE',  ( -0.000000000000000000, -0.000000000000000000, -1.000000000000000000 ) ) ;
#3054 = ORIENTED_EDGE ( 'NONE', *, *, #688, .T. ) ;
#3055 = PERSON_AND_ORGANIZATION ( #7862, #8117 ) ;
#3056 = LINE ( 'NONE', #6215, #7693 ) ;
#3057 = ORGANIZATION ( 'NAUO-ORG8', 'UNSPECIFIED', 'UNSPECIFIED' ) ;
#3058 = DATE_AND_TIME ( #557, #7284 ) ;
#3059 = LINE ( 'NONE', #3793, #3105 ) ;
#3060 = AXIS2_PLACEMENT_3D ( 'NONE', #1131, #6128, #7658 ) ;
#3061 = VECTOR ( 'NONE', #5932, 39.37007874015748143 ) ;
#3062 =( GEOMETRIC_REPRESENTATION_CONTEXT ( 3 ) GLOBAL_UNCERTAINTY_ASSIGNED_CONTEXT ( ( #7025 ) ) GLOBAL_UNIT_ASSIGNED_CONTEXT ( ( #2479, #6402, #3127 ) ) REPRESENTATION_CONTEXT ( 'NONE', 'WORKASPACE' ) );
#3063 = CARTESIAN_POINT ( 'NONE',  ( 1.624999999999999556, 2.076218724953421191, -2.749999999536766992 ) ) ;
#3064 = DIRECTION ( 'NONE',  ( 1.000000000000000000, 0.000000000000000000, 0.000000000000000000 ) ) ;
#3065 = AXIS2_PLACEMENT_3D ( 'NONE', #5871, #1362, #3849 ) ;
#3066 = CYLINDRICAL_SURFACE ( 'NONE', #7936, 2.845000000000001528 ) ;
#3067 = ORIENTED_EDGE ( 'NONE', *, *, #3977, .T. ) ;
#3068 = CARTESIAN_POINT ( 'NONE',  ( -0.6956352003900579950, 4.230470471097700802, 8.091948598562707318 ) ) ;
#3069 = AXIS2_PLACEMENT_3D ( 'NONE', #5884, #3342, #842 ) ;
#3070 =( NAMED_UNIT ( * ) PLANE_ANGLE_UNIT ( ) SI_UNIT ( $, .RADIAN. ) );
#3071 = CC_DESIGN_PERSON_AND_ORGANIZATION_ASSIGNMENT ( #3867, #1461, ( #1491 ) ) ;
#3072 = PLANE ( 'NONE',  #5283 ) ;
#3073 = DIRECTION ( 'NONE',  ( -1.000000000000000000, 0.000000000000000000, 0.000000000000000000 ) ) ;
#3074 = PERSON_AND_ORGANIZATION ( #7862, #8117 ) ;
#3075 = ORIENTED_EDGE ( 'NONE', *, *, #1821, .T. ) ;
#3076 = DIRECTION ( 'NONE',  ( 0.000000000000000000, 0.7071067811865475727, -0.7071067811865475727 ) ) ;
#3077 = AXIS2_PLACEMENT_3D ( 'NONE', #5350, #939, #3522 ) ;
#3078 = AXIS2_PLACEMENT_3D ( 'NONE', #3173, #229, #1986 ) ;
#3079 = DIRECTION ( 'NONE',  ( -0.000000000000000000, 1.000000000000000000, 0.000000000000000000 ) ) ;
#3080 = PRODUCT_DEFINITION_SHAPE ( 'NONE', 'NONE',  #8190 ) ;
#3081 = ORIENTED_EDGE ( 'NONE', *, *, #1581, .T. ) ;
#3082 = EDGE_CURVE ( 'NONE', #3479, #5810, #434, .T. ) ;
#3083 = DIMENSIONAL_EXPONENTS ( 1.000000000000000000, 0.000000000000000000, 0.000000000000000000, 0.000000000000000000, 0.000000000000000000, 0.000000000000000000, 0.000000000000000000 ) ;
#3084 = CARTESIAN_POINT ( 'NONE',  ( 0.8969582018468957862, 2.990857292758699160, -5.108750000000002345 ) ) ;
#3085 = DIRECTION ( 'NONE',  ( 0.000000000000000000, 0.000000000000000000, 1.000000000000000000 ) ) ;
#3086 = DIRECTION ( 'NONE',  ( 0.000000000000000000, 0.000000000000000000, 1.000000000000000000 ) ) ;
#3087 = CARTESIAN_POINT ( 'NONE',  ( -2.740000000000000213, 8.719000000000001194, 3.823750000000002647 ) ) ;
#3088 = EDGE_CURVE ( 'NONE', #4445, #8018, #707, .T. ) ;
#3089 = VECTOR ( 'NONE', #4405, 39.37007874015748854 ) ;
#3090 = ORIENTED_EDGE ( 'NONE', *, *, #3243, .T. ) ;
#3091 = ORIENTED_EDGE ( 'NONE', *, *, #3819, .T. ) ;
#3092 = AXIS2_PLACEMENT_3D ( 'NONE', #7897, #7809, #4649 ) ;
#3093 = CIRCLE ( 'NONE', #72, 0.3124999879509117728 ) ;
#3094 = DIRECTION ( 'NONE',  ( -0.000000000000000000, 0.000000000000000000, -1.000000000000000000 ) ) ;
#3095 = CARTESIAN_POINT ( 'NONE',  ( -2.740000000000000213, 8.719000000000001194, 3.323750000000001759 ) ) ;
#3096 = EDGE_CURVE ( 'NONE', #3668, #5577, #1851, .T. ) ;
#3097 = FACE_OUTER_BOUND ( 'NONE', #2394, .T. ) ;
#3098 =( BOUNDED_CURVE ( )  B_SPLINE_CURVE ( 3, ( #3320, #2713, #4424, #3201 ),
 .UNSPECIFIED., .F., .T. ) 
 B_SPLINE_CURVE_WITH_KNOTS ( ( 4, 4 ),
 ( 0.000000000000000000, 0.09428240746600526079 ),
 .UNSPECIFIED. ) 
 CURVE ( )  GEOMETRIC_REPRESENTATION_ITEM ( )  RATIONAL_B_SPLINE_CURVE ( ( 1.000000000000000000, 0.3333333333333330373, 0.3333333333333330373, 1.000000000000000000 ) ) 
 REPRESENTATION_ITEM ( '' )  );
#3099 = ORIENTED_EDGE ( 'NONE', *, *, #6849, .T. ) ;
#3100 = PERSON_AND_ORGANIZATION ( #7862, #8117 ) ;
#3101 = DIRECTION ( 'NONE',  ( -0.000000000000000000, 1.000000000000000000, -0.000000000000000000 ) ) ;
#3102 = VECTOR ( 'NONE', #4154, 39.37007874015748143 ) ;
#3103 = VERTEX_POINT ( 'NONE', #4684 ) ;
#3104 = EDGE_CURVE ( 'NONE', #822, #6945, #3506, .T. ) ;
#3105 = VECTOR ( 'NONE', #1267, 39.37007874015748143 ) ;
#3106 = CARTESIAN_POINT ( 'NONE',  ( -2.375000000000003109, 5.137500000000000178, 6.956249999999992717 ) ) ;
#3107 = ORIENTED_EDGE ( 'NONE', *, *, #1821, .F. ) ;
#3108 = COORDINATED_UNIVERSAL_TIME_OFFSET ( 0, 0, .AHEAD. ) ;
#3109 = CARTESIAN_POINT ( 'NONE',  ( 2.740000000000001545, 7.964000000000000412, 3.823750000000002647 ) ) ;
#3110 = PERSON_AND_ORGANIZATION ( #8170, #4056 ) ;
#3111 = CARTESIAN_POINT ( 'NONE',  ( 0.7335700393700786970, 2.500000000000000444, 0.5625000000000001110 ) ) ;
#3112 = LINE ( 'NONE', #5604, #2911 ) ;
#3113 = FACE_OUTER_BOUND ( 'NONE', #6816, .T. ) ;
#3114 = DIRECTION ( 'NONE',  ( -0.000000000000000000, 0.000000000000000000, 1.000000000000000000 ) ) ;
#3115 = CARTESIAN_POINT ( 'NONE',  ( 1.462953684860233805, 1.000000000000000666, 3.588229579187919960 ) ) ;
#3116 = ORIENTED_EDGE ( 'NONE', *, *, #337, .F. ) ;
#3117 = CARTESIAN_POINT ( 'NONE',  ( -4.462046614173229564, 3.753500037802127043, 8.231249998505111520 ) ) ;
#3118 = EDGE_CURVE ( 'NONE', #7757, #3161, #5656, .T. ) ;
#3119 =( NAMED_UNIT ( * ) SI_UNIT ( $, .STERADIAN. ) SOLID_ANGLE_UNIT ( ) );
#3120 = CARTESIAN_POINT ( 'NONE',  ( -3.362499999999999822, 1.750000000000000222, 6.725000000000002309 ) ) ;
#3121 = CARTESIAN_POINT ( 'NONE',  ( 4.476342532109287120, 3.950000015938371689, 7.918750010554200358 ) ) ;
#3122 = SHAPE_DEFINITION_REPRESENTATION ( #4249, #6505 ) ;
#3123 = VERTEX_POINT ( 'NONE', #2448 ) ;
#3124 = LINE ( 'NONE', #7618, #5842 ) ;
#3125 = CC_DESIGN_PERSON_AND_ORGANIZATION_ASSIGNMENT ( #6843, #1843, ( #6424 ) ) ;
#3126 = DIRECTION ( 'NONE',  ( -1.000000000000000000, 0.000000000000000000, 0.000000000000000000 ) ) ;
#3127 =( NAMED_UNIT ( * ) SI_UNIT ( $, .STERADIAN. ) SOLID_ANGLE_UNIT ( ) );
#3128 = ORIENTED_EDGE ( 'NONE', *, *, #4927, .T. ) ;
#3129 = ORIENTED_EDGE ( 'NONE', *, *, #943, .T. ) ;
#3130 = EDGE_CURVE ( 'NONE', #1364, #5899, #593, .T. ) ;
#3131 = CARTESIAN_POINT ( 'NONE',  ( 0.000000000000000000, 5.639000000000001123, 0.1249999999999997641 ) ) ;
#3132 = CARTESIAN_POINT ( 'NONE',  ( 1.136188160977859019, 3.292580994510421633, -5.108750000000003233 ) ) ;
#3133 = CARTESIAN_POINT ( 'NONE',  ( 0.000000000000000000, 1.749999999911819204, 0.000000000000000000 ) ) ;
#3134 = ORIENTED_EDGE ( 'NONE', *, *, #3020, .T. ) ;
#3135 = APPROVAL_ROLE ( '' ) ;
#3136 = DIRECTION ( 'NONE',  ( 0.000000000000000000, 0.000000000000000000, 1.000000000000000000 ) ) ;
#3137 = EDGE_CURVE ( 'NONE', #3703, #2223, #2966, .T. ) ;
#3138 = ORIENTED_EDGE ( 'NONE', *, *, #5023, .T. ) ;
#3139 = EDGE_CURVE ( 'NONE', #3411, #5813, #165, .T. ) ;
#3140 = DIRECTION ( 'NONE',  ( -0.5773502691896257311, -0.5773502691896257311, 0.5773502691896257311 ) ) ;
#3141 = CARTESIAN_POINT ( 'NONE',  ( 1.187500000000000444, 7.339000000000003965, 4.267772478794107371 ) ) ;
#3142 = CARTESIAN_POINT ( 'NONE',  ( -1.172489671586610882, 1.365923996832131609E-16, -3.693357951819908891 ) ) ;
#3143 = ORIENTED_EDGE ( 'NONE', *, *, #1970, .F. ) ;
#3144 = PERSON_AND_ORGANIZATION_ROLE ( 'creator' ) ;
#3145 = CARTESIAN_POINT ( 'NONE',  ( 1.198957881890679422, 2.500000000000000000, 2.749999999536767437 ) ) ;
#3146 = CALENDAR_DATE ( 2026, 8, 10 ) ;
#3147 = APPLICATION_CONTEXT ( 'configuration controlled 3d designs of mechanical parts and assemblies' ) ;
#3148 = CARTESIAN_POINT ( 'NONE',  ( -3.987046614173228587, 3.792944682095130027, 8.112380013461466532 ) ) ;
#3149 = CARTESIAN_POINT ( 'NONE',  ( 2.750000000000000444, 8.719000000000002970, 3.823750000000002647 ) ) ;
#3150 = CARTESIAN_POINT ( 'NONE',  ( 2.537499998660271761, 3.550000000000001155, -1.169467086614173645 ) ) ;
#3151 = ORIENTED_EDGE ( 'NONE', *, *, #2865, .T. ) ;
#3152 = DIRECTION ( 'NONE',  ( 0.000000000000000000, -1.000000000000000000, 0.000000000000000000 ) ) ;
#3153 =( CONVERSION_BASED_UNIT ( 'INCH', #3688 ) LENGTH_UNIT ( ) NAMED_UNIT ( #624 ) );
#3154 = DIRECTION ( 'NONE',  ( -0.000000000000000000, 1.000000000000000000, 0.000000000000000000 ) ) ;
#3155 = PERSON_AND_ORGANIZATION ( #7862, #8117 ) ;
#3156 = EDGE_LOOP ( 'NONE', ( #3515, #5568, #5309 ) ) ;
#3157 = LINE ( 'NONE', #1353, #4413 ) ;
#3158 = FACE_OUTER_BOUND ( 'NONE', #912, .T. ) ;
#3159 = CARTESIAN_POINT ( 'NONE',  ( 3.987953385826772390, 4.146499994074615003, 8.231249998505111520 ) ) ;
#3160 = PLANE ( 'NONE',  #580 ) ;
#3161 = VERTEX_POINT ( 'NONE', #3029 ) ;
#3162 = ORIENTED_EDGE ( 'NONE', *, *, #7670, .T. ) ;
#3163 = EDGE_CURVE ( 'NONE', #3439, #7577, #4307, .T. ) ;
#3164 = CARTESIAN_POINT ( 'NONE',  ( 3.987953385826771946, 4.130262297440340014, 8.152751440554144580 ) ) ;
#3165 = CARTESIAN_POINT ( 'NONE',  ( 1.044888736288899667, 4.748860047246612481, -5.108750000000002345 ) ) ;
#3166 = LINE ( 'NONE', #511, #3609 ) ;
#3167 = ORIENTED_EDGE ( 'NONE', *, *, #7634, .T. ) ;
#3168 = CALENDAR_DATE ( 2026, 8, 10 ) ;
#3169 = DIRECTION ( 'NONE',  ( -1.000000000000000000, 0.000000000000000000, 0.000000000000000000 ) ) ;
#3170 = ORIENTED_EDGE ( 'NONE', *, *, #2746, .T. ) ;
#3171 = ADVANCED_FACE ( 'NONE', ( #1695 ), #8141, .T. ) ;
#3172 = VECTOR ( 'NONE', #3586, 39.37007874015748143 ) ;
#3173 = CARTESIAN_POINT ( 'NONE',  ( -8.751021560936518753E-10, 1.365923996832131609E-16, 5.750408897959578548E-10 ) ) ;
#3174 = CARTESIAN_POINT ( 'NONE',  ( 1.187500000000000444, 7.964000000000000412, 5.236250000000000071 ) ) ;
#3175 = DIRECTION ( 'NONE',  ( 1.000000000000000000, 0.000000000000000000, 0.000000000000000000 ) ) ;
#3176 = VECTOR ( 'NONE', #3981, 39.37007874015748143 ) ;
#3177 = VERTEX_POINT ( 'NONE', #4175 ) ;
#3178 = CALENDAR_DATE ( 2026, 8, 10 ) ;
#3179 = CIRCLE ( 'NONE', #2264, 3.874999999025058539 ) ;
#3180 = EDGE_CURVE ( 'NONE', #1857, #2109, #2006, .T. ) ;
#3181 = DIRECTION ( 'NONE',  ( 0.5773502691896257311, 0.5773502691896257311, 0.5773502691896257311 ) ) ;
#3182 = CC_DESIGN_SECURITY_CLASSIFICATION ( #2137, ( #1491 ) ) ;
#3183 = APPROVAL_STATUS ( 'not_yet_approved' ) ;
#3184 = CYLINDRICAL_SURFACE ( 'NONE', #1875, 1.249999999999999556 ) ;
#3185 = CARTESIAN_POINT ( 'NONE',  ( 0.6827599196736722220, 3.639582871947503850, 8.189746072949246170 ) ) ;
#3186 = VECTOR ( 'NONE', #1697, 39.37007874015748143 ) ;
#3187 = VECTOR ( 'NONE', #4492, 39.37007874015748143 ) ;
#3188 = CARTESIAN_POINT ( 'NONE',  ( -3.987046614173228587, 3.856588441154243263, 8.058147833247129910 ) ) ;
#3189 = CARTESIAN_POINT ( 'NONE',  ( 0.000000000000000000, 3.950000000000000178, -2.750000000000000444 ) ) ;
#3190 = FACE_OUTER_BOUND ( 'NONE', #3634, .T. ) ;
#3191 = ORIENTED_EDGE ( 'NONE', *, *, #3330, .T. ) ;
#3192 = CARTESIAN_POINT ( 'NONE',  ( -3.987046614173229031, 3.753500037802126599, 8.624249954777603477 ) ) ;
#3193 = CARTESIAN_POINT ( 'NONE',  ( 0.000000000000000000, 0.000000000000000000, 0.000000000000000000 ) ) ;
#3194 = CARTESIAN_POINT ( 'NONE',  ( -3.562500000000000444, 0.000000000000000000, 2.975000000000000977 ) ) ;
#3195 = AXIS2_PLACEMENT_3D ( 'NONE', #7473, #3884, #4428 ) ;
#3196 = PERSON_AND_ORGANIZATION_ROLE ( 'design_owner' ) ;
#3197 = ORIENTED_EDGE ( 'NONE', *, *, #4218, .F. ) ;
#3198 = AXIS2_PLACEMENT_3D ( 'NONE', #107, #5643, #6310 ) ;
#3199 = CARTESIAN_POINT ( 'NONE',  ( -1.500000000000000444, 5.113999999999999879, -2.750000000000000444 ) ) ;
#3200 = CIRCLE ( 'NONE', #4104, 0.1875000000000006661 ) ;
#3201 = CARTESIAN_POINT ( 'NONE',  ( 0.000000000000000000, 2.762500000000000178, 6.956250000000000711 ) ) ;
#3202 = CARTESIAN_POINT ( 'NONE',  ( 1.500000000000000444, 5.414000000000000590, 0.5414159055118110686 ) ) ;
#3203 = CARTESIAN_POINT ( 'NONE',  ( 0.000000000000000000, 3.950000000000000178, 6.956250000000000711 ) ) ;
#3204 = ORIENTED_EDGE ( 'NONE', *, *, #3280, .T. ) ;
#3205 = ORIENTED_EDGE ( 'NONE', *, *, #1082, .T. ) ;
#3206 = CARTESIAN_POINT ( 'NONE',  ( 3.987953385826771946, 3.757075529380056622, 8.193927407620869019 ) ) ;
#3207 = VECTOR ( 'NONE', #1627, 39.37007874015748143 ) ;
#3208 = CARTESIAN_POINT ( 'NONE',  ( 1.295380378688662182, 4.162394200796177834, -5.108750000000002345 ) ) ;
#3209 = CARTESIAN_POINT ( 'NONE',  ( -1.500000000000000444, 5.339000000000000412, -2.750000000000000444 ) ) ;
#3210 = VERTEX_POINT ( 'NONE', #2605 ) ;
#3211 = EDGE_CURVE ( 'NONE', #4886, #7925, #3179, .T. ) ;
#3212 = LINE ( 'NONE', #716, #5714 ) ;
#3213 = ORIENTED_EDGE ( 'NONE', *, *, #3118, .T. ) ;
#3214 = AXIS2_PLACEMENT_3D ( 'NONE', #3705, #5466, #7935 ) ;
#3215 = APPROVAL ( #637, 'UNSPECIFIED' ) ;
#3216 = CARTESIAN_POINT ( 'NONE',  ( -1.201750196850394081, 2.500000000000000444, 0.5625000000000003331 ) ) ;
#3217 = CARTESIAN_POINT ( 'NONE',  ( 3.182000000000000828, 2.359000000000000874, 3.956250000000000266 ) ) ;
#3218 = DIRECTION ( 'NONE',  ( -0.000000000000000000, 1.000000000000000000, 0.000000000000000000 ) ) ;
#3219 = VECTOR ( 'NONE', #1806, 39.37007874015748143 ) ;
#3220 = ORIENTED_EDGE ( 'NONE', *, *, #4471, .F. ) ;
#3221 = VECTOR ( 'NONE', #2919, 39.37007874015748143 ) ;
#3222 = PERSON_AND_ORGANIZATION_ROLE ( 'creator' ) ;
#3223 = CARTESIAN_POINT ( 'NONE',  ( -2.740000000000000657, 7.964000000000000412, 3.333750000000001990 ) ) ;
#3224 = LINE ( 'NONE', #4946, #2060 ) ;
#3225 = AXIS2_PLACEMENT_3D ( 'NONE', #3471, #3995, #353 ) ;
#3226 = VERTEX_POINT ( 'NONE', #225 ) ;
#3227 = LINE ( 'NONE', #1342, #1098 ) ;
#3228 = DIRECTION ( 'NONE',  ( 0.000000000000000000, 0.000000000000000000, 1.000000000000000000 ) ) ;
#3229 = ORIENTED_EDGE ( 'NONE', *, *, #4877, .F. ) ;
#3230 = CARTESIAN_POINT ( 'NONE',  ( -4.066213280839896527, 4.383999996532201848, 8.231249998505111520 ) ) ;
#3231 =( NAMED_UNIT ( * ) PLANE_ANGLE_UNIT ( ) SI_UNIT ( $, .RADIAN. ) );
#3232 = FACE_OUTER_BOUND ( 'NONE', #4788, .T. ) ;
#3233 = CARTESIAN_POINT ( 'NONE',  ( 2.750000000000000444, 8.719000000000002970, 4.313750000000002416 ) ) ;
#3234 = PERSON_AND_ORGANIZATION_ROLE ( 'classification_officer' ) ;
#3235 = AXIS2_PLACEMENT_3D ( 'NONE', #788, #5783, #871 ) ;
#3236 = VERTEX_POINT ( 'NONE', #2150 ) ;
#3237 = LINE ( 'NONE', #4504, #7037 ) ;
#3238 =( BOUNDED_CURVE ( )  B_SPLINE_CURVE ( 3, ( #3874, #6348, #194, #6307 ),
 .UNSPECIFIED., .F., .F. ) 
 B_SPLINE_CURVE_WITH_KNOTS ( ( 4, 4 ),
 ( 0.000000000000000000, 0.03896959999066340607 ),
 .UNSPECIFIED. ) 
 CURVE ( )  GEOMETRIC_REPRESENTATION_ITEM ( )  RATIONAL_B_SPLINE_CURVE ( ( 0.5678235990678962564, 0.5416270346111723422, 0.5230192003173261828, 0.5120000961863576672 ) ) 
 REPRESENTATION_ITEM ( '' )  );
#3239 = CARTESIAN_POINT ( 'NONE',  ( 2.875000000000000888, 1.000000000000000222, -3.337500001222715174 ) ) ;
#3240 = FACE_OUTER_BOUND ( 'NONE', #6935, .T. ) ;
#3241 = FACE_OUTER_BOUND ( 'NONE', #6173, .T. ) ;
#3242 = EDGE_CURVE ( 'NONE', #4502, #3161, #2072, .T. ) ;
#3243 = EDGE_CURVE ( 'NONE', #811, #3703, #2405, .T. ) ;
#3244 = ORIENTED_EDGE ( 'NONE', *, *, #1810, .F. ) ;
#3245 = B_SPLINE_CURVE_WITH_KNOTS ( 'NONE', 3,
 ( #7263, #1641, #4124, #6177 ),
 .UNSPECIFIED., .F., .F.,
 ( 4, 4 ),
 ( 0.000000000000000000, 0.01222568465131274387 ),
 .UNSPECIFIED. ) ;
#3246 = ORIENTED_EDGE ( 'NONE', *, *, #5184, .T. ) ;
#3247 = CARTESIAN_POINT ( 'NONE',  ( 3.987953385826772834, 3.767882598671357552, 8.157439729585936661 ) ) ;
#3248 = CARTESIAN_POINT ( 'NONE',  ( 0.3427223730929865875, 5.219860580395915051, -5.108749999999999680 ) ) ;
#3249 = CARTESIAN_POINT ( 'NONE',  ( 0.6796608066838680795, 2.472726760981024174, -2.935416550745896469 ) ) ;
#3250 = CYLINDRICAL_SURFACE ( 'NONE', #3993, 1.624999995942718156 ) ;
#3251 = EDGE_CURVE ( 'NONE', #7586, #6784, #1580, .T. ) ;
#3252 = VERTEX_POINT ( 'NONE', #250 ) ;
#3253 = CARTESIAN_POINT ( 'NONE',  ( 3.987953385826772834, 3.801472271119643143, 8.360613120147613486 ) ) ;
#3254 = ORIENTED_EDGE ( 'NONE', *, *, #878, .T. ) ;
#3255 = PRODUCT ( 'bench vise9-', 'bench vise9-', '', ( #6611 ) ) ;
#3256 = SHAPE_REPRESENTATION ( 'MAS-412', ( #6361, #4510, #2163, #6745, #5561, #4248, #1249, #7840, #858, #7567 ), #1001 ) ;
#3257 = FACE_OUTER_BOUND ( 'NONE', #3738, .T. ) ;
#3258 = DIRECTION ( 'NONE',  ( 0.000000000000000000, 0.000000000000000000, -1.000000000000000000 ) ) ;
#3259 = EDGE_LOOP ( 'NONE', ( #1894, #2175, #8174, #2937, #469, #4704, #2101, #4422 ) ) ;
#3260 = APPROVAL_STATUS ( 'not_yet_approved' ) ;
#3261 = CARTESIAN_POINT ( 'NONE',  ( 2.750000000000000444, 8.719000000000002970, 4.313750000000002416 ) ) ;
#3262 = ITEM_DEFINED_TRANSFORMATION ( 'NONE', 'NONE', #3853,  #7272 ) ;
#3263 = CARTESIAN_POINT ( 'NONE',  ( 0.7499999999999995559, 3.929104627039257558, 7.918749999999998401 ) ) ;
#3264 = APPROVAL ( #4318, 'UNSPECIFIED' ) ;
#3265 = DIRECTION ( 'NONE',  ( 0.000000000000000000, 1.000000000000000000, 0.000000000000000000 ) ) ;
#3266 = CARTESIAN_POINT ( 'NONE',  ( 0.000000000000000000, 2.500000000000000000, 0.000000000000000000 ) ) ;
#3267 = VERTEX_POINT ( 'NONE', #5233 ) ;
#3268 = EDGE_CURVE ( 'NONE', #7262, #3887, #2783, .T. ) ;
#3269 = CARTESIAN_POINT ( 'NONE',  ( -2.750000000000000888, 7.974000000000001087, 3.823750000000002647 ) ) ;
#3270 = CARTESIAN_POINT ( 'NONE',  ( -2.750000000000000444, 8.574153543168254288, 4.323749999249341336 ) ) ;
#3271 = CARTESIAN_POINT ( 'NONE',  ( -3.987046614173229919, 4.023056220426558305, 8.413666033243972109 ) ) ;
#3272 = ORIENTED_EDGE ( 'NONE', *, *, #2339, .T. ) ;
#3273 = DIRECTION ( 'NONE',  ( -1.000000000000000000, 0.000000000000000000, 0.000000000000000000 ) ) ;
#3274 = CARTESIAN_POINT ( 'NONE',  ( -1.187500000000000222, 4.913650942705939606, 4.937346008500399286 ) ) ;
#3275 = CARTESIAN_POINT ( 'NONE',  ( 2.750000000000000888, 7.974000000000001087, 3.333750000000001990 ) ) ;
#3276 = PERSON_AND_ORGANIZATION ( #7862, #8117 ) ;
#3277 = ORIENTED_EDGE ( 'NONE', *, *, #538, .F. ) ;
#3278 = B_SPLINE_CURVE_WITH_KNOTS ( 'NONE', 3,
 ( #1933, #6275, #626, #8143, #8184, #3159 ),
 .UNSPECIFIED., .F., .F.,
 ( 4, 2, 4 ),
 ( 0.000000000000000000, 0.5000000000000000000, 1.000000000000000000 ),
 .UNSPECIFIED. ) ;
#3279 = ADVANCED_FACE ( 'NONE', ( #6577 ), #3316, .T. ) ;
#3280 = EDGE_CURVE ( 'NONE', #6942, #95, #2173, .T. ) ;
#3281 = DIRECTION ( 'NONE',  ( 0.000000000000000000, 0.000000000000000000, -1.000000000000000000 ) ) ;
#3282 = FACE_BOUND ( 'NONE', #653, .T. ) ;
#3283 = FACE_OUTER_BOUND ( 'NONE', #2242, .T. ) ;
#3284 = EDGE_LOOP ( 'NONE', ( #5257, #7845, #4930, #5874, #5, #3297 ) ) ;
#3285 = EDGE_CURVE ( 'NONE', #7385, #5858, #6651, .T. ) ;
#3286 = CARTESIAN_POINT ( 'NONE',  ( -0.6889980206436411292, 3.653596005017110127, 8.130130038714286300 ) ) ;
#3287 = ORIENTED_EDGE ( 'NONE', *, *, #1538, .T. ) ;
#3288 =( BOUNDED_CURVE ( )  B_SPLINE_CURVE ( 3, ( #6903, #5542, #2560, #3042 ),
 .UNSPECIFIED., .F., .F. ) 
 B_SPLINE_CURVE_WITH_KNOTS ( ( 4, 4 ),
 ( 0.000000000000000000, 0.03896959986073553206 ),
 .UNSPECIFIED. ) 
 CURVE ( )  GEOMETRIC_REPRESENTATION_ITEM ( )  RATIONAL_B_SPLINE_CURVE ( ( 0.7490764964646237090, 0.6867990767679545971, 0.6362002288929724525, 0.5972799528396776081 ) ) 
 REPRESENTATION_ITEM ( '' )  );
#3289 = EDGE_CURVE ( 'NONE', #6623, #1945, #1746, .T. ) ;
#3290 = CARTESIAN_POINT ( 'NONE',  ( 3.987953385826771946, 4.051974939361221217, 8.063149917160938429 ) ) ;
#3291 = CARTESIAN_POINT ( 'NONE',  ( 0.6588840751933063844, 5.085949231003589865, -5.108749999999999680 ) ) ;
#3292 = DIRECTION ( 'NONE',  ( 1.000000000000000000, 0.000000000000000000, 0.000000000000000000 ) ) ;
#3293 = ORIENTED_EDGE ( 'NONE', *, *, #2689, .F. ) ;
#3294 = ADVANCED_FACE ( 'NONE', ( #4127, #3360, #1643 ), #206, .T. ) ;
#3295 = CARTESIAN_POINT ( 'NONE',  ( -1.312500000000000444, 4.908106850393701315, 2.749999992430256945 ) ) ;
#3296 = LINE ( 'NONE', #7204, #2943 ) ;
#3297 = ORIENTED_EDGE ( 'NONE', *, *, #2725, .T. ) ;
#3298 = DATE_AND_TIME ( #6420, #7397 ) ;
#3299 = DIRECTION ( 'NONE',  ( 0.9917930140139563644, 0.000000000000000000, -0.1278538906451900103 ) ) ;
#3300 = ITEM_DEFINED_TRANSFORMATION ( 'NONE', 'NONE', #3727,  #7272 ) ;
#3301 = DIRECTION ( 'NONE',  ( 0.000000000000000000, -1.000000000000000000, 0.000000000000000000 ) ) ;
#3302 = LINE ( 'NONE', #3350, #6898 ) ;
#3303 = ORIENTED_EDGE ( 'NONE', *, *, #6123, .T. ) ;
#3304 = VECTOR ( 'NONE', #1006, 39.37007874015748143 ) ;
#3305 = CARTESIAN_POINT ( 'NONE',  ( -3.987046614173229475, 4.037524053340656671, 8.055097764145708439 ) ) ;
#3306 = CC_DESIGN_DATE_AND_TIME_ASSIGNMENT ( #2115, #4608, ( #1882 ) ) ;
#3307 = CC_DESIGN_APPROVAL ( #2224, ( #1622 ) ) ;
#3308 = CARTESIAN_POINT ( 'NONE',  ( -3.987046614173229475, 3.761880377346255244, 8.288651076800222839 ) ) ;
#3309 = EDGE_LOOP ( 'NONE', ( #3866, #4073, #2961, #1124 ) ) ;
#3310 = PLANE ( 'NONE',  #7411 ) ;
#3311 = EDGE_LOOP ( 'NONE', ( #861, #7235, #3385, #3777 ) ) ;
#3312 = DIRECTION ( 'NONE',  ( 1.000000000000000000, 0.000000000000000000, 0.000000000000000000 ) ) ;
#3313 = CARTESIAN_POINT ( 'NONE',  ( -2.750000000000000444, 7.531471846334603981, 3.944609322583843891 ) ) ;
#3314 = CALENDAR_DATE ( 2026, 8, 10 ) ;
#3315 = EDGE_LOOP ( 'NONE', ( #6185, #4621, #3566, #6069 ) ) ;
#3316 = CYLINDRICAL_SURFACE ( 'NONE', #2794, 0.1875000000000006661 ) ;
#3317 = AXIS2_PLACEMENT_3D ( 'NONE', #3830, #6219, #610 ) ;
#3318 = APPROVAL_PERSON_ORGANIZATION ( #3388, #7812, #7207 ) ;
#3319 = CC_DESIGN_PERSON_AND_ORGANIZATION_ASSIGNMENT ( #6750, #5009, ( #2668 ) ) ;
#3320 = CARTESIAN_POINT ( 'NONE',  ( 0.000000000000000000, 5.137500000000000178, 6.956250000000000711 ) ) ;
#3321 = CARTESIAN_POINT ( 'NONE',  ( 2.750000000000000444, 8.589000000000000412, 2.411250000000000338 ) ) ;
#3322 = VECTOR ( 'NONE', #5365, 39.37007874015748143 ) ;
#3323 = LENGTH_MEASURE_WITH_UNIT ( LENGTH_MEASURE( 0.02539999999999999897 ), #6442 );
#3324 = CARTESIAN_POINT ( 'NONE',  ( 2.537500000000000533, 2.500000000000000444, -0.2625000000000008438 ) ) ;
#3325 = PERSON_AND_ORGANIZATION_ROLE ( 'design_supplier' ) ;
#3326 = ORIENTED_EDGE ( 'NONE', *, *, #7196, .F. ) ;
#3327 = DIRECTION ( 'NONE',  ( 0.000000000000000000, -1.000000000000000000, 0.000000000000000000 ) ) ;
#3328 = CARTESIAN_POINT ( 'NONE',  ( 0.7333924044284377830, 3.792775136080777987, 8.501510692915044132 ) ) ;
#3329 = VECTOR ( 'NONE', #3960, 39.37007874015748143 ) ;
#3330 = EDGE_CURVE ( 'NONE', #2504, #5232, #6852, .T. ) ;
#3331 = DIRECTION ( 'NONE',  ( 0.000000000000000000, 0.000000000000000000, 1.000000000000000000 ) ) ;
#3332 = CARTESIAN_POINT ( 'NONE',  ( 4.067120052493439886, 4.383999996532200960, 7.363250037317452090 ) ) ;
#3333 = VECTOR ( 'NONE', #5116, 39.37007874015748854 ) ;
#3334 = DIRECTION ( 'NONE',  ( -0.000000000000000000, -1.000000000000000000, -0.000000000000000000 ) ) ;
#3335 = VECTOR ( 'NONE', #7173, 39.37007874015748143 ) ;
#3336 = ORIENTED_EDGE ( 'NONE', *, *, #6938, .F. ) ;
#3337 = FACE_OUTER_BOUND ( 'NONE', #7325, .T. ) ;
#3338 = ORIENTED_EDGE ( 'NONE', *, *, #4109, .T. ) ;
#3339 = VECTOR ( 'NONE', #5096, 39.37007874015748143 ) ;
#3340 = CC_DESIGN_SECURITY_CLASSIFICATION ( #600, ( #8196 ) ) ;
#3341 = DIRECTION ( 'NONE',  ( 1.000000000000000000, 0.000000000000000000, 0.000000000000000000 ) ) ;
#3342 = DIRECTION ( 'NONE',  ( 0.7071067811865475727, -0.7071067811865475727, 0.000000000000000000 ) ) ;
#3343 = ORIENTED_EDGE ( 'NONE', *, *, #4218, .T. ) ;
#3344 = APPROVAL_DATE_TIME ( #5851, #5120 ) ;
#3345 = DIRECTION ( 'NONE',  ( -1.000000000000000000, -0.000000000000000000, -0.000000000000000000 ) ) ;
#3346 = ADVANCED_FACE ( 'N', ( #3405 ), #5517, .T. ) ;
#3347 = PERSON_AND_ORGANIZATION_ROLE ( 'classification_officer' ) ;
#3348 = DIRECTION ( 'NONE',  ( -0.000000000000000000, 0.000000000000000000, -1.000000000000000000 ) ) ;
#3349 = VECTOR ( 'NONE', #2569, 39.37007874015748143 ) ;
#3350 = CARTESIAN_POINT ( 'NONE',  ( -2.750000000000000444, 8.729000000000002757, 4.313750000000002416 ) ) ;
#3351 = DIRECTION ( 'NONE',  ( 0.000000000000000000, -0.7071067811865475727, 0.7071067811865475727 ) ) ;
#3352 = VERTEX_POINT ( 'NONE', #6836 ) ;
#3353 = EDGE_CURVE ( 'NONE', #4996, #3433, #1183, .T. ) ;
#3354 = CARTESIAN_POINT ( 'NONE',  ( -3.987046614173228587, 3.799477730093518080, 8.357885377186541120 ) ) ;
#3355 = ORIENTED_EDGE ( 'NONE', *, *, #1778, .F. ) ;
#3356 = CARTESIAN_POINT ( 'NONE',  ( 3.796513186599489220, 1.000000000000000444, -2.946478861041413211 ) ) ;
#3357 = CARTESIAN_POINT ( 'NONE',  ( -2.078417272059708142E-11, 5.414000000000000590, 2.749999998413802160 ) ) ;
#3358 = APPROVAL_ROLE ( '' ) ;
#3359 = ORIENTED_EDGE ( 'NONE', *, *, #19, .F. ) ;
#3360 = FACE_BOUND ( 'NONE', #7819, .T. ) ;
#3361 = CARTESIAN_POINT ( 'NONE',  ( 0.7052155605301346775, 5.414000000000000590, 0.000000000000000000 ) ) ;
#3362 = FACE_OUTER_BOUND ( 'NONE', #4830, .T. ) ;
#3363 = VECTOR ( 'NONE', #7882, 39.37007874015748854 ) ;
#3364 = PLANE ( 'NONE',  #3065 ) ;
#3365 = VERTEX_POINT ( 'NONE', #3650 ) ;
#3366 = SHAPE_DEFINITION_REPRESENTATION ( #769, #578 ) ;
#3367 = ORIENTED_EDGE ( 'NONE', *, *, #1662, .T. ) ;
#3368 = CARTESIAN_POINT ( 'NONE',  ( 0.000000000000000000, 1.749999999911819204, -3.343750000040417447 ) ) ;
#3369 = CARTESIAN_POINT ( 'NONE',  ( 0.7253895767696342256, 3.758660869344151223, 8.479158915174224376 ) ) ;
#3370 = CC_DESIGN_PERSON_AND_ORGANIZATION_ASSIGNMENT ( #7144, #7880, ( #7674 ) ) ;
#3371 = EDGE_CURVE ( 'NONE', #2528, #5154, #1218, .T. ) ;
#3372 = DIRECTION ( 'NONE',  ( -0.3026345437736693289, 0.000000000000000000, 0.9531066744677130220 ) ) ;
#3373 = CARTESIAN_POINT ( 'NONE',  ( 4.462953385826771147, 4.146499994074615891, 8.231249998505111520 ) ) ;
#3374 = DIRECTION ( 'NONE',  ( 0.000000000000000000, 0.000000000000000000, -1.000000000000000000 ) ) ;
#3375 = VERTEX_POINT ( 'NONE', #8083 ) ;
#3376 = CARTESIAN_POINT ( 'NONE',  ( -3.651126736336024692, 1.000000000000000444, -1.298036422402331302 ) ) ;
#3377 = CARTESIAN_POINT ( 'NONE',  ( -0.7253671533374044245, 3.759190173666904666, 8.478940687276063315 ) ) ;
#3378 = VERTEX_POINT ( 'NONE', #5564 ) ;
#3379 = APPROVAL_PERSON_ORGANIZATION ( #2215, #1365, #3358 ) ;
#3380 = EDGE_CURVE ( 'NONE', #4179, #4298, #6721, .T. ) ;
#3381 = SECURITY_CLASSIFICATION ( '', '', #5231 ) ;
#3382 = EDGE_CURVE ( 'NONE', #1162, #7981, #6145, .T. ) ;
#3383 = EDGE_CURVE ( 'NONE', #2271, #7545, #1109, .T. ) ;
#3384 = DIRECTION ( 'NONE',  ( -0.9961332539796342589, 0.000000000000000000, -0.08785522361217638909 ) ) ;
#3385 = ORIENTED_EDGE ( 'NONE', *, *, #3180, .T. ) ;
#3386 = PERSON_AND_ORGANIZATION ( #7862, #8117 ) ;
#3387 = CARTESIAN_POINT ( 'NONE',  ( -3.687499989627467389, 1.000000000000000888, 3.874999999790589289 ) ) ;
#3388 = PERSON_AND_ORGANIZATION ( #5052, #3057 ) ;
#3389 = CARTESIAN_POINT ( 'NONE',  ( 0.7491290119348462673, 3.908602837234293581, 7.920824285553323740 ) ) ;
#3390 = LINE ( 'NONE', #803, #2714 ) ;
#3391 = PLANE ( 'NONE',  #3225 ) ;
#3392 = EDGE_CURVE ( 'NONE', #5031, #5123, #3527, .T. ) ;
#3393 = ORIENTED_EDGE ( 'NONE', *, *, #4691, .F. ) ;
#3394 = EDGE_CURVE ( 'NONE', #605, #4681, #3943, .T. ) ;
#3395 = CARTESIAN_POINT ( 'NONE',  ( 0.000000000000000000, 5.510994133858271304, 4.968462007874015818 ) ) ;
#3396 = CARTESIAN_POINT ( 'NONE',  ( -3.987046614173228143, 4.027703970067585182, 8.411747167338614162 ) ) ;
#3397 = VERTEX_POINT ( 'NONE', #5438 ) ;
#3398 = CARTESIAN_POINT ( 'NONE',  ( -2.740000000000001545, 7.964000000000000412, 3.823750000000002647 ) ) ;
#3399 = ORIENTED_EDGE ( 'NONE', *, *, #7579, .T. ) ;
#3400 = FACE_OUTER_BOUND ( 'NONE', #2041, .T. ) ;
#3401 = CARTESIAN_POINT ( 'NONE',  ( 1.249999999999999556, 3.950000000000000178, 3.691250000234376660 ) ) ;
#3402 = APPLICATION_PROTOCOL_DEFINITION ( 'international standard', 'config_control_design', 1994, #5547 ) ;
#3403 = ORIENTED_EDGE ( 'NONE', *, *, #2928, .F. ) ;
#3404 = B_SPLINE_CURVE_WITH_KNOTS ( 'NONE', 3,
 ( #5934, #357, #5264, #5227 ),
 .UNSPECIFIED., .F., .F.,
 ( 4, 4 ),
 ( 0.000000000000000000, 0.01222568467003884961 ),
 .UNSPECIFIED. ) ;
#3405 = FACE_OUTER_BOUND ( 'NONE', #6771, .T. ) ;
#3406 = CARTESIAN_POINT ( 'NONE',  ( -1.625000000000000222, 5.113999999999999879, 2.750000000000000444 ) ) ;
#3407 =( BOUNDED_SURFACE ( )  B_SPLINE_SURFACE ( 3, 3, ( 
 ( #8150, #3432, #542, #1823 ),
 ( #4314, #7336, #7377, #8063 ),
 ( #2485, #1705, #3040, #594 ),
 ( #4969, #3631, #7510, #2398 ) ),
 .UNSPECIFIED., .F., .F., .T. ) 
 B_SPLINE_SURFACE_WITH_KNOTS ( ( 4, 4 ),
 ( 4, 4 ),
 ( 0.000000000000000000, 1.000000000000000000 ),
 ( 0.000000000000000000, 1.000000000000000000 ),
 .UNSPECIFIED. ) 
 GEOMETRIC_REPRESENTATION_ITEM ( )  RATIONAL_B_SPLINE_SURFACE ( (
 ( 1.000000000000000000, 0.4766096016200470631, 0.4766096016200470631, 1.000000000000000000),
 ( 0.6249252401552001235, 0.2978453697526821098, 0.2978453697526821098, 0.6249252401552001235),
 ( 0.6249252401552001235, 0.2978453697526821098, 0.2978453697526821098, 0.6249252401552001235),
 ( 1.000000000000000000, 0.4766096016200470631, 0.4766096016200470631, 1.000000000000000000) ) ) 
 REPRESENTATION_ITEM ( '' )  SURFACE ( )  );
#3408 = DIRECTION ( 'NONE',  ( -1.000000000000000000, 0.000000000000000000, -0.000000000000000000 ) ) ;
#3409 = ORIENTED_EDGE ( 'NONE', *, *, #4090, .F. ) ;
#3410 = PERSON_AND_ORGANIZATION_ROLE ( 'creator' ) ;
#3411 = VERTEX_POINT ( 'NONE', #3683 ) ;
#3412 = PLANE ( 'NONE',  #2840 ) ;
#3413 = SECURITY_CLASSIFICATION ( '', '', #2301 ) ;
#3414 = FACE_OUTER_BOUND ( 'NONE', #6483, .T. ) ;
#3415 = APPROVAL ( #6873, 'UNKNOWN' ) ;
#3416 = CARTESIAN_POINT ( 'NONE',  ( 3.987953385826771946, 4.146499994074616779, 7.838250042232624892 ) ) ;
#3417 = CARTESIAN_POINT ( 'NONE',  ( 3.987953385826772834, 4.142615650101508784, 8.270135292618689959 ) ) ;
#3418 = ORIENTED_EDGE ( 'NONE', *, *, #3749, .T. ) ;
#3419 = EDGE_CURVE ( 'NONE', #2413, #2164, #5171, .T. ) ;
#3420 = CC_DESIGN_APPROVAL ( #7812, ( #1197 ) ) ;
#3421 = PLANE ( 'NONE',  #1910 ) ;
#3422 = CARTESIAN_POINT ( 'NONE',  ( 2.537500000000000533, 2.500000000000000444, 0.4312500000000004663 ) ) ;
#3423 = FACE_OUTER_BOUND ( 'NONE', #5534, .T. ) ;
#3424 = PERSON_AND_ORGANIZATION ( #7862, #8117 ) ;
#3425 = DIRECTION ( 'NONE',  ( 0.000000000000000000, 1.000000000000000000, -0.000000000000000000 ) ) ;
#3426 = COORDINATED_UNIVERSAL_TIME_OFFSET ( 0, 0, .AHEAD. ) ;
#3427 = LINE ( 'NONE', #847, #1618 ) ;
#3428 = CARTESIAN_POINT ( 'NONE',  ( 0.7491290119348464893, 3.991397162765705442, 8.541675714446673950 ) ) ;
#3429 = ADVANCED_FACE ( 'NONE', ( #494 ), #4330, .T. ) ;
#3430 = ORIENTED_EDGE ( 'NONE', *, *, #2084, .F. ) ;
#3431 = EDGE_CURVE ( 'NONE', #941, #7817, #4913, .T. ) ;
#3432 = CARTESIAN_POINT ( 'NONE',  ( 0.1186214960629921461, 5.264455944881891725, -5.098178543307088972 ) ) ;
#3433 = VERTEX_POINT ( 'NONE', #4295 ) ;
#3434 = DIRECTION ( 'NONE',  ( -0.000000000000000000, 1.000000000000000000, -0.000000000000000000 ) ) ;
#3435 = ORIENTED_EDGE ( 'NONE', *, *, #7374, .T. ) ;
#3436 = DIRECTION ( 'NONE',  ( 0.0005594472316430793100, -2.733119188255727182E-17, 0.9999998435093852001 ) ) ;
#3437 = DIRECTION ( 'NONE',  ( -0.000000000000000000, 1.000000000000000000, -0.000000000000000000 ) ) ;
#3438 = APPROVAL_ROLE ( '' ) ;
#3439 = VERTEX_POINT ( 'NONE', #3063 ) ;
#3440 = CARTESIAN_POINT ( 'NONE',  ( -0.08551597065243228546, 5.262577827926121721, -5.108750000000001457 ) ) ;
#3441 = LOCAL_TIME ( 0, 37, 23.00000000000000000, #6300 ) ;
#3442 = CARTESIAN_POINT ( 'NONE',  ( -1.044888770141576328, 3.151139990177239447, -5.108750000000002345 ) ) ;
#3443 = CARTESIAN_POINT ( 'NONE',  ( 0.06423988825481448395, 2.326186878295140481, 3.079038241297371137 ) ) ;
#3444 = LINE ( 'NONE', #3406, #2806 ) ;
#3445 = DIRECTION ( 'NONE',  ( -0.000000000000000000, -1.000000000000000000, 0.000000000000000000 ) ) ;
#3446 = APPROVAL_ROLE ( '' ) ;
#3447 = ORIENTED_EDGE ( 'NONE', *, *, #5083, .T. ) ;
#3448 = VECTOR ( 'NONE', #5068, 39.37007874015748854 ) ;
#3449 = CARTESIAN_POINT ( 'NONE',  ( -1.624999999999999778, 3.950000000000000178, -5.108750000000001457 ) ) ;
#3450 = APPROVAL_PERSON_ORGANIZATION ( #598, #7131, #6905 ) ;
#3451 = AXIS2_PLACEMENT_3D ( 'NONE', #7842, #7923, #2260 ) ;
#3452 = CIRCLE ( 'NONE', #7541, 1.249999999999999556 ) ;
#3453 = LOCAL_TIME ( 0, 37, 23.00000000000000000, #2813 ) ;
#3454 = DIRECTION ( 'NONE',  ( -0.000000000000000000, -1.000000000000000000, -0.000000000000000000 ) ) ;
#3455 = CARTESIAN_POINT ( 'NONE',  ( 4.067120052493439886, 4.383999996532201848, 8.231249998505111520 ) ) ;
#3456 = CARTESIAN_POINT ( 'NONE',  ( 3.987953385826771946, 4.140928214022170373, 8.277905906474343212 ) ) ;
#3457 = VECTOR ( 'NONE', #3666, 39.37007874015748143 ) ;
#3458 = ORIENTED_EDGE ( 'NONE', *, *, #7872, .F. ) ;
#3459 = AXIS2_PLACEMENT_3D ( 'NONE', #581, #3126, #3085 ) ;
#3460 = CIRCLE ( 'NONE', #2021, 3.874999999025058539 ) ;
#3461 = FACE_OUTER_BOUND ( 'NONE', #5073, .T. ) ;
#3462 = DIRECTION ( 'NONE',  ( -1.000000000000000000, 0.000000000000000000, 0.000000000000000000 ) ) ;
#3463 = VECTOR ( 'NONE', #1635, 39.37007874015748143 ) ;
#3464 = AXIS2_PLACEMENT_3D ( 'NONE', #8144, #4756, #1123 ) ;
#3465 = CARTESIAN_POINT ( 'NONE',  ( 0.3224709391354322330, 2.356032306969389367, -3.049642098122674838 ) ) ;
#3466 = CARTESIAN_POINT ( 'NONE',  ( -3.343750000000001776, 0.000000000000000000, 0.000000000000000000 ) ) ;
#3467 = ORIENTED_EDGE ( 'NONE', *, *, #441, .T. ) ;
#3468 = PERSON_AND_ORGANIZATION ( #7862, #8117 ) ;
#3469 = CARTESIAN_POINT ( 'NONE',  ( 1.625000000000000222, 5.113999999999999879, -2.750000000000000444 ) ) ;
#3470 = CARTESIAN_POINT ( 'NONE',  ( 0.7078558382242214897, 4.198166876146032678, 8.422262045139364162 ) ) ;
#3471 = CARTESIAN_POINT ( 'NONE',  ( 0.000000000000000000, 5.151388682096968097, 2.750000000000000444 ) ) ;
#3472 = VECTOR ( 'NONE', #569, 39.37007874015748143 ) ;
#3473 = CARTESIAN_POINT ( 'NONE',  ( 2.750000000000002665, 8.589000000000000412, 3.243476614173228967 ) ) ;
#3474 = CC_DESIGN_PERSON_AND_ORGANIZATION_ASSIGNMENT ( #6090, #1668, ( #2798 ) ) ;
#3475 =( GEOMETRIC_REPRESENTATION_CONTEXT ( 3 ) GLOBAL_UNCERTAINTY_ASSIGNED_CONTEXT ( ( #1451 ) ) GLOBAL_UNIT_ASSIGNED_CONTEXT ( ( #3612, #8088, #371 ) ) REPRESENTATION_CONTEXT ( 'NONE', 'WORKASPACE' ) );
#3476 = VERTEX_POINT ( 'NONE', #6799 ) ;
#3477 = CARTESIAN_POINT ( 'NONE',  ( -2.537500000000000533, 1.664000000000000368, -0.2625000000000008438 ) ) ;
#3478 = VECTOR ( 'NONE', #5763, 39.37007874015748854 ) ;
#3479 = VERTEX_POINT ( 'NONE', #563 ) ;
#3480 = DIRECTION ( 'NONE',  ( 0.000000000000000000, 0.000000000000000000, -1.000000000000000000 ) ) ;
#3481 = CARTESIAN_POINT ( 'NONE',  ( 4.462953385826771147, 4.146499994074615891, 8.231249998505111520 ) ) ;
#3482 = ORIENTED_EDGE ( 'NONE', *, *, #2542, .F. ) ;
#3483 = AXIS2_PLACEMENT_3D ( 'NONE', #5059, #7598, #1949 ) ;
#3484 = SECURITY_CLASSIFICATION_LEVEL ( 'unclassified' ) ;
#3485 = CARTESIAN_POINT ( 'NONE',  ( 0.000000000000000000, 5.536672282146935409, 4.083473622047245399 ) ) ;
#3486 = PERSON_AND_ORGANIZATION ( #7862, #8117 ) ;
#3487 = ORIENTED_EDGE ( 'NONE', *, *, #1245, .F. ) ;
#3488 = CARTESIAN_POINT ( 'NONE',  ( -3.562500000000000444, -3.820994442221351629E-18, 3.337500000000003020 ) ) ;
#3489 = CARTESIAN_POINT ( 'NONE',  ( -1.291725147455078382, 3.716413631672734752, -5.108749999999998792 ) ) ;
#3490 = CARTESIAN_POINT ( 'NONE',  ( 0.2590873717497497175, 2.344476708467012394, 3.061018729179389997 ) ) ;
#3491 = DIRECTION ( 'NONE',  ( -1.000000000000000000, 0.000000000000000000, 0.000000000000000000 ) ) ;
#3492 = CARTESIAN_POINT ( 'NONE',  ( 2.745000000000000995, 7.973999999999999311, 4.318750000000002309 ) ) ;
#3493 = APPROVAL_STATUS ( 'not_yet_approved' ) ;
#3494 = VECTOR ( 'NONE', #2331, 39.37007874015748854 ) ;
#3495 = ORIENTED_EDGE ( 'NONE', *, *, #5272, .T. ) ;
#3496 = LINE ( 'NONE', #5488, #7168 ) ;
#3497 = LINE ( 'NONE', #6000, #3322 ) ;
#3498 = ADVANCED_FACE ( 'NONE', ( #8128 ), #2466, .T. ) ;
#3499 = EDGE_CURVE ( 'NONE', #750, #7757, #6025, .T. ) ;
#3500 = DIRECTION ( 'NONE',  ( 0.000000000000000000, -0.000000000000000000, 1.000000000000000000 ) ) ;
#3501 = FACE_OUTER_BOUND ( 'NONE', #3810, .T. ) ;
#3502 = VERTEX_POINT ( 'NONE', #1685 ) ;
#3503 =( BOUNDED_CURVE ( )  B_SPLINE_CURVE ( 3, ( #2657, #2614, #6600, #7250 ),
 .UNSPECIFIED., .F., .F. ) 
 B_SPLINE_CURVE_WITH_KNOTS ( ( 4, 4 ),
 ( 0.000000000000000000, 0.04204456198606273953 ),
 .UNSPECIFIED. ) 
 CURVE ( )  GEOMETRIC_REPRESENTATION_ITEM ( )  RATIONAL_B_SPLINE_CURVE ( ( 1.000000000000000000, 0.9998483700553054687, 0.9997031153252196045, 0.9995642358097424074 ) ) 
 REPRESENTATION_ITEM ( '' )  );
#3504 = CARTESIAN_POINT ( 'NONE',  ( -3.987046614173228587, 4.093738155682585145, 8.097094170350759512 ) ) ;
#3505 = LINE ( 'NONE', #4103, #3221 ) ;
#3506 = LINE ( 'NONE', #7202, #6460 ) ;
#3507 = ADVANCED_FACE ( 'NONE', ( #6685 ), #1069, .T. ) ;
#3508 = CARTESIAN_POINT ( 'NONE',  ( 3.987953385826772390, 4.146499994074615003, 8.231249998505111520 ) ) ;
#3509 = DIRECTION ( 'NONE',  ( -0.7071067811865475727, 0.000000000000000000, -0.7071067811865475727 ) ) ;
#3510 = EDGE_LOOP ( 'NONE', ( #7556, #3399, #1825, #7048 ) ) ;
#3511 = APPROVAL_STATUS ( 'not_yet_approved' ) ;
#3512 = CARTESIAN_POINT ( 'NONE',  ( 2.750000000000000444, 7.964000000000000412, 3.691250000000001030 ) ) ;
#3513 = CARTESIAN_POINT ( 'NONE',  ( 0.6956352003900579950, 4.230470471097700802, 8.370551401437293038 ) ) ;
#3514 = CARTESIAN_POINT ( 'NONE',  ( 1.312500000000000444, 7.339000000000003077, 2.411250000000000782 ) ) ;
#3515 = ORIENTED_EDGE ( 'NONE', *, *, #5901, .T. ) ;
#3516 = CARTESIAN_POINT ( 'NONE',  ( 0.000000000000000000, 1.749999999911819204, 0.000000000000000000 ) ) ;
#3517 = EDGE_LOOP ( 'NONE', ( #6292, #161, #5716, #5314 ) ) ;
#3518 = FACE_OUTER_BOUND ( 'NONE', #3980, .T. ) ;
#3519 = EDGE_LOOP ( 'NONE', ( #7711, #5494, #3254, #385 ) ) ;
#3520 = DATE_AND_TIME ( #6714, #5698 ) ;
#3521 = PRODUCT_DEFINITION ( 'UNKNOWN', '', #1877, #7625 ) ;
#3522 = DIRECTION ( 'NONE',  ( 1.000000000000000000, 0.000000000000000000, 0.000000000000000000 ) ) ;
#3523 = SECURITY_CLASSIFICATION_LEVEL ( 'unclassified' ) ;
#3524 = ORIENTED_EDGE ( 'NONE', *, *, #1, .F. ) ;
#3525 = FACE_OUTER_BOUND ( 'NONE', #2881, .T. ) ;
#3526 = EDGE_CURVE ( 'NONE', #805, #7672, #2946, .T. ) ;
#3527 = LINE ( 'NONE', #7398, #5402 ) ;
#3528 = DIRECTION ( 'NONE',  ( -0.7071067811865474617, 0.000000000000000000, 0.7071067811865474617 ) ) ;
#3529 = CARTESIAN_POINT ( 'NONE',  ( -3.987046614173228587, 4.146499994074616779, 8.231249998505111520 ) ) ;
#3530 = APPLICATION_PROTOCOL_DEFINITION ( 'international standard', 'config_control_design', 1994, #6515 ) ;
#3531 = ORIENTED_EDGE ( 'NONE', *, *, #1977, .F. ) ;
#3532 = DIRECTION ( 'NONE',  ( -0.000000000000000000, 1.000000000000000000, 0.000000000000000000 ) ) ;
#3533 = EDGE_CURVE ( 'NONE', #822, #402, #5769, .T. ) ;
#3534 = DIRECTION ( 'NONE',  ( -0.7071067811865475727, 0.7071067811865475727, 0.000000000000000000 ) ) ;
#3535 = DIRECTION ( 'NONE',  ( 1.000000000000000000, -1.016501579037865957E-15, 0.000000000000000000 ) ) ;
#3536 = EDGE_CURVE ( 'NONE', #987, #6365, #7003, .T. ) ;
#3537 = CARTESIAN_POINT ( 'NONE',  ( -2.875000000000000888, 1.000000000000000222, -2.612499998777286780 ) ) ;
#3538 = DIRECTION ( 'NONE',  ( 0.000000000000000000, -0.000000000000000000, 1.000000000000000000 ) ) ;
#3539 = ORIENTED_EDGE ( 'NONE', *, *, #3708, .F. ) ;
#3540 = CARTESIAN_POINT ( 'NONE',  ( -3.987046614173228587, 3.962486853702869016, 8.034748693519857099 ) ) ;
#3541 = DIRECTION ( 'NONE',  ( 0.000000000000000000, 0.000000000000000000, 1.000000000000000000 ) ) ;
#3542 = FACE_OUTER_BOUND ( 'NONE', #5949, .T. ) ;
#3543 = CARTESIAN_POINT ( 'NONE',  ( -2.740000000000001545, 8.729000000000002757, 4.313750000000002416 ) ) ;
#3544 = ORIENTED_EDGE ( 'NONE', *, *, #6740, .T. ) ;
#3545 = COORDINATED_UNIVERSAL_TIME_OFFSET ( 0, 0, .AHEAD. ) ;
#3546 = DIRECTION ( 'NONE',  ( 0.000000000000000000, 0.000000000000000000, -1.000000000000000000 ) ) ;
#3547 = CARTESIAN_POINT ( 'NONE',  ( -2.740000000000001545, 7.964000000000000412, 3.833750000000001545 ) ) ;
#3548 = ADVANCED_FACE ( 'NONE', ( #3113 ), #15, .T. ) ;
#3549 = EDGE_CURVE ( 'NONE', #4517, #2229, #3227, .T. ) ;
#3550 = ORIENTED_EDGE ( 'NONE', *, *, #7046, .F. ) ;
#3551 = DIRECTION ( 'NONE',  ( 0.9925485533564400997, 0.000000000000000000, -0.1218497814115311745 ) ) ;
#3552 = ORIENTED_EDGE ( 'NONE', *, *, #5998, .F. ) ;
#3553 = DIRECTION ( 'NONE',  ( -1.000000000000000000, 0.000000000000000000, 0.000000000000000000 ) ) ;
#3554 = ORIENTED_EDGE ( 'NONE', *, *, #1381, .F. ) ;
#3555 = COORDINATED_UNIVERSAL_TIME_OFFSET ( 0, 0, .AHEAD. ) ;
#3556 = CARTESIAN_POINT ( 'NONE',  ( 3.987953385826771946, 4.225666661560476101, 8.231249998505111520 ) ) ;
#3557 = DIRECTION ( 'NONE',  ( 0.000000000000000000, -1.000000000000000000, 0.000000000000000000 ) ) ;
#3558 = SECURITY_CLASSIFICATION_LEVEL ( 'unclassified' ) ;
#3559 = ORIENTED_EDGE ( 'NONE', *, *, #5549, .F. ) ;
#3560 = B_SPLINE_CURVE_WITH_KNOTS ( 'NONE', 3,
 ( #84, #3742, #4395, #1415, #713, #3814, #1982, #2067, #4558, #5710, #1248, #1372, #6244, #2599, #3084, #5624, #634, #5127, #7590, #3132, #4514, #5006, #2518, #3857, #6940, #6326, #7549, #122, #1943, #6902, #3892, #1290, #5091, #5660, #3208, #3780, #6284, #4432, #2640, #6369, #755, #668, #792, #7629, #3165, #7713, #1326, #38, #2559, #7667, #5049, #3291, #4470, #6983, #5789, #3248, #5753, #2020, #7030, #6411, #168 ),
 .UNSPECIFIED., .F., .F.,
 ( 4, 2, 2, 2, 2, 2, 2, 2, 2, 2, 2, 1, 2, 2, 2, 2, 2, 2, 2, 2, 2, 2, 2, 2, 2, 2, 2, 2, 2, 2, 4 ),
 ( 0.1042068716910059117, 0.1107198011716938740, 0.1139762659120378552, 0.1172327306523818502, 0.1237456601330697986, 0.1253738925032417961, 0.1270021248734137798, 0.1302585896137577470, 0.1367715190944456816, 0.1383997514646176930, 0.1400279838347896766, 0.1432844485751335883, 0.1465409133154775279, 0.1481691456856495115, 0.1497973780558214951, 0.1563103075365094574, 0.1595667722768534524, 0.1611950046470254361, 0.1628232370171974197, 0.1693361664978854098, 0.1709643988680573656, 0.1725926312382293215, 0.1758490959785732333, 0.1823620254592609458, 0.1856184901996048298, 0.1888749549399486583, 0.1921314196802925145, 0.1953878844206363707, 0.2019008139013241110, 0.2051572786416679672, 0.2084137433820118235 ),
 .UNSPECIFIED. ) ;
#3561 = CARTESIAN_POINT ( 'NONE',  ( 0.000000000000000000, 5.151388682096968097, -2.749999999536767437 ) ) ;
#3562 = CARTESIAN_POINT ( 'NONE',  ( -0.7499999999999995559, 3.970887754116599666, 8.543750000000002842 ) ) ;
#3563 = SHAPE_REPRESENTATION_RELATIONSHIP ( 'NONE' , 'NONE' ,  #6969, #549 ) ;
#3564 = CARTESIAN_POINT ( 'NONE',  ( 1.312500000184909199, 4.908106857043937232, 3.316250000000001030 ) ) ;
#3565 = DATE_AND_TIME ( #7405, #7327 ) ;
#3566 = ORIENTED_EDGE ( 'NONE', *, *, #2551, .T. ) ;
#3567 = APPLICATION_CONTEXT ( 'configuration controlled 3d designs of mechanical parts and assemblies' ) ;
#3568 = DIRECTION ( 'NONE',  ( 1.000000000000000000, 0.000000000000000000, 0.000000000000000000 ) ) ;
#3569 = DESIGN_CONTEXT ( 'detailed design', #2926, 'design' ) ;
#3570 = SHAPE_REPRESENTATION ( 'bench vise6-', ( #5158, #7560, #3853, #3727 ), #50 ) ;
#3571 = CC_DESIGN_PERSON_AND_ORGANIZATION_ASSIGNMENT ( #3386, #232, ( #2483 ) ) ;
#3572 = LINE ( 'NONE', #4018, #309 ) ;
#3573 = CIRCLE ( 'NONE', #432, 0.6000000000000015321 ) ;
#3574 = AXIS2_PLACEMENT_3D ( 'NONE', #4948, #7490, #1838 ) ;
#3575 = DIRECTION ( 'NONE',  ( -1.000000000000000000, -0.000000000000000000, -0.000000000000000000 ) ) ;
#3576 = LOCAL_TIME ( 0, 37, 23.00000000000000000, #1548 ) ;
#3577 = CARTESIAN_POINT ( 'NONE',  ( 2.375000000000000888, 5.137500000000001066, 6.956249999999999822 ) ) ;
#3578 = VERTEX_POINT ( 'NONE', #6957 ) ;
#3579 = DIRECTION ( 'NONE',  ( -0.000000000000000000, -1.000000000000000000, -0.000000000000000000 ) ) ;
#3580 = ORIENTED_EDGE ( 'NONE', *, *, #6831, .F. ) ;
#3581 = VECTOR ( 'NONE', #297, 39.37007874015748143 ) ;
#3582 = EDGE_CURVE ( 'NONE', #2355, #6986, #733, .T. ) ;
#3583 = LOCAL_TIME ( 0, 37, 23.00000000000000000, #4553 ) ;
#3584 = CARTESIAN_POINT ( 'NONE',  ( -3.987046614173227699, 3.876943811449999888, 8.048833963766311328 ) ) ;
#3585 = CARTESIAN_POINT ( 'NONE',  ( 0.000000000000000000, 1.750000000000000666, -3.343750000000000444 ) ) ;
#3586 = DIRECTION ( 'NONE',  ( -0.000000000000000000, 0.000000000000000000, 1.000000000000000000 ) ) ;
#3587 = AXIS2_PLACEMENT_3D ( 'NONE', #5420, #543, #5541 ) ;
#3588 = CARTESIAN_POINT ( 'NONE',  ( -3.791570908345035740, 1.000000000000000222, 0.7997593681799637366 ) ) ;
#3589 = ORIENTED_EDGE ( 'NONE', *, *, #3082, .T. ) ;
#3590 = DATE_AND_TIME ( #2363, #1356 ) ;
#3591 = VECTOR ( 'NONE', #6028, 39.37007874015748143 ) ;
#3592 = DIRECTION ( 'NONE',  ( -0.000000000000000000, 1.000000000000000000, -0.000000000000000000 ) ) ;
#3593 = CARTESIAN_POINT ( 'NONE',  ( 1.312500000000000222, 7.964000000000000412, 2.411250000000000338 ) ) ;
#3594 = AXIS2_PLACEMENT_3D ( 'NONE', #7185, #6581, #5360 ) ;
#3595 = ORIENTED_EDGE ( 'NONE', *, *, #6291, .F. ) ;
#3596 = CIRCLE ( 'NONE', #3464, 1.074999999999999289 ) ;
#3597 = DIRECTION ( 'NONE',  ( -0.000000000000000000, -0.000000000000000000, 1.000000000000000000 ) ) ;
#3598 = DIRECTION ( 'NONE',  ( -0.000000000000000000, -0.000000000000000000, 1.000000000000000000 ) ) ;
#3599 = EDGE_CURVE ( 'NONE', #6568, #2664, #2673, .T. ) ;
#3600 = VERTEX_POINT ( 'NONE', #1994 ) ;
#3601 = COORDINATED_UNIVERSAL_TIME_OFFSET ( 0, 0, .AHEAD. ) ;
#3602 = DIRECTION ( 'NONE',  ( -0.000000000000000000, -1.000000000000000000, -0.000000000000000000 ) ) ;
#3603 = VECTOR ( 'NONE', #4381, 39.37007874015748143 ) ;
#3604 = PERSON_AND_ORGANIZATION ( #2444, #6033 ) ;
#3605 = ORIENTED_EDGE ( 'NONE', *, *, #7546, .T. ) ;
#3606 = CARTESIAN_POINT ( 'NONE',  ( -1.187500000000000000, 8.523567361455139491, 4.820336051656679999 ) ) ;
#3607 = CARTESIAN_POINT ( 'NONE',  ( -2.637478091534712021, 0.9999999999981570298, -2.843572666449250441 ) ) ;
#3608 = DIRECTION ( 'NONE',  ( -0.7071067811865282549, -0.7071067811865668906, 0.000000000000000000 ) ) ;
#3609 = VECTOR ( 'NONE', #40, 39.37007874015748143 ) ;
#3610 = APPROVAL_PERSON_ORGANIZATION ( #5135, #1862, #1424 ) ;
#3611 = CARTESIAN_POINT ( 'NONE',  ( -0.7210596466522595227, 4.156871429633926418, 8.466341326185078842 ) ) ;
#3612 =( CONVERSION_BASED_UNIT ( 'INCH', #4300 ) LENGTH_UNIT ( ) NAMED_UNIT ( #6273 ) );
#3613 = CARTESIAN_POINT ( 'NONE',  ( 2.513411990276540831, 1.000000000000000222, -2.949302488239232023 ) ) ;
#3614 = CC_DESIGN_APPROVAL ( #2066, ( #600 ) ) ;
#3615 = DATE_AND_TIME ( #6805, #3795 ) ;
#3616 = ORIENTED_EDGE ( 'NONE', *, *, #5286, .T. ) ;
#3617 = CARTESIAN_POINT ( 'NONE',  ( 3.583510604133039124, 1.543025754838326824, -7.167021208266083576 ) ) ;
#3618 = DIRECTION ( 'NONE',  ( 0.000000000000000000, 0.000000000000000000, -1.000000000000000000 ) ) ;
#3619 = VECTOR ( 'NONE', #5883, 39.37007874015748143 ) ;
#3620 = VERTEX_POINT ( 'NONE', #2501 ) ;
#3621 = LINE ( 'NONE', #7503, #5406 ) ;
#3622 = VECTOR ( 'NONE', #4584, 39.37007874015748143 ) ;
#3623 = CARTESIAN_POINT ( 'NONE',  ( 2.749999999999998668, 7.339000000000003077, 5.236250000000000071 ) ) ;
#3624 = EDGE_LOOP ( 'NONE', ( #6120, #4219, #4402, #6052, #6346, #5583 ) ) ;
#3625 = CC_DESIGN_PERSON_AND_ORGANIZATION_ASSIGNMENT ( #4258, #6691, ( #1419 ) ) ;
#3626 = LINE ( 'NONE', #4270, #6845 ) ;
#3627 = VERTEX_POINT ( 'NONE', #7569 ) ;
#3628 = VECTOR ( 'NONE', #7353, 39.37007874015748143 ) ;
#3629 = EDGE_CURVE ( 'NONE', #295, #2186, #4622, .T. ) ;
#3630 = DIRECTION ( 'NONE',  ( -0.000000000000000000, -0.000000000000000000, 1.000000000000000000 ) ) ;
#3631 = CARTESIAN_POINT ( 'NONE',  ( 0.6696957874015749823, 2.330452401574803822, -5.651700944881890010 ) ) ;
#3632 = CARTESIAN_POINT ( 'NONE',  ( 2.750000000000000444, 7.964000000000000412, 3.691250000000001030 ) ) ;
#3633 = CARTESIAN_POINT ( 'NONE',  ( 1.187500000000000222, 4.232796286020916732, 6.817001420565361514 ) ) ;
#3634 = EDGE_LOOP ( 'NONE', ( #3933, #6853, #5841, #7040 ) ) ;
#3635 = COORDINATED_UNIVERSAL_TIME_OFFSET ( 0, 0, .AHEAD. ) ;
#3636 = DIRECTION ( 'NONE',  ( 0.000000000000000000, 0.000000000000000000, -1.000000000000000000 ) ) ;
#3637 = ADVANCED_FACE ( 'NONE', ( #4538 ), #1219, .F. ) ;
#3638 = ORIENTED_EDGE ( 'NONE', *, *, #6036, .F. ) ;
#3639 = EDGE_CURVE ( 'NONE', #2678, #7297, #838, .T. ) ;
#3640 = PLANE ( 'NONE',  #6373 ) ;
#3641 = CARTESIAN_POINT ( 'NONE',  ( -4.382879947506562068, 4.383999996532200960, 8.231249998505111520 ) ) ;
#3642 = ORIENTED_EDGE ( 'NONE', *, *, #1193, .T. ) ;
#3643 = APPROVAL_DATE_TIME ( #7259, #6229 ) ;
#3644 = EDGE_CURVE ( 'NONE', #1601, #231, #4848, .T. ) ;
#3645 = CARTESIAN_POINT ( 'NONE',  ( 4.383786719160105427, 3.516000035344544639, 9.099249959692768286 ) ) ;
#3646 = CARTESIAN_POINT ( 'NONE',  ( -0.5808953455350218675, 5.130091789537773117, -5.108750000000001457 ) ) ;
#3647 = APPROVAL_DATE_TIME ( #7261, #8075 ) ;
#3648 = CARTESIAN_POINT ( 'NONE',  ( -1.187499999717754884, 7.436775081331068016, 4.083473622121677415 ) ) ;
#3649 = DIRECTION ( 'NONE',  ( -0.000000000000000000, -0.000000000000000000, -1.000000000000000000 ) ) ;
#3650 = CARTESIAN_POINT ( 'NONE',  ( -2.740000000000001545, 7.973999999999999311, 3.823750000000002647 ) ) ;
#3651 = CARTESIAN_POINT ( 'NONE',  ( -2.750000000000000444, 7.964000000000000412, 3.691250000000001030 ) ) ;
#3652 = ORIENTED_EDGE ( 'NONE', *, *, #4375, .F. ) ;
#3653 = CARTESIAN_POINT ( 'NONE',  ( -0.7253895767696344477, 4.141339130655848244, 8.479158915174227928 ) ) ;
#3654 = DIRECTION ( 'NONE',  ( -0.5773502691896258421, 0.5773502691896258421, 0.5773502691896258421 ) ) ;
#3655 = PERSON_AND_ORGANIZATION_ROLE ( 'design_supplier' ) ;
#3656 = VERTEX_POINT ( 'NONE', #7200 ) ;
#3657 = EDGE_CURVE ( 'NONE', #4253, #7385, #1702, .T. ) ;
#3658 = ORIENTED_EDGE ( 'NONE', *, *, #4476, .T. ) ;
#3659 = CARTESIAN_POINT ( 'NONE',  ( 2.537500000000000533, 2.500000000000000444, 0.000000000000000000 ) ) ;
#3660 = DIRECTION ( 'NONE',  ( 0.000000000000000000, 0.000000000000000000, -1.000000000000000000 ) ) ;
#3661 = ORIENTED_EDGE ( 'NONE', *, *, #538, .T. ) ;
#3662 = ORIENTED_EDGE ( 'NONE', *, *, #7992, .T. ) ;
#3663 = CC_DESIGN_PERSON_AND_ORGANIZATION_ASSIGNMENT ( #1388, #6998, ( #5167 ) ) ;
#3664 = DIRECTION ( 'NONE',  ( 0.000000000000000000, 0.000000000000000000, -1.000000000000000000 ) ) ;
#3665 = CARTESIAN_POINT ( 'NONE',  ( -3.987046614173228143, 3.754593536049172453, 8.255194476360108169 ) ) ;
#3666 = DIRECTION ( 'NONE',  ( -0.000000000000000000, -1.000000000000000000, 0.000000000000000000 ) ) ;
#3667 = CARTESIAN_POINT ( 'NONE',  ( 1.187499999999999112, 4.849232312069990947, 5.299003540426529213 ) ) ;
#3668 = VERTEX_POINT ( 'NONE', #4184 ) ;
#3669 = SHAPE_DEFINITION_REPRESENTATION ( #7354, #5548 ) ;
#3670 = CARTESIAN_POINT ( 'NONE',  ( -2.750000000000000444, 7.521783346446682117, 3.691250000461920866 ) ) ;
#3671 = ADVANCED_FACE ( 'NONE', ( #3461 ), #7049, .F. ) ;
#3672 = CC_DESIGN_SECURITY_CLASSIFICATION ( #1832, ( #8187 ) ) ;
#3673 = CC_DESIGN_PERSON_AND_ORGANIZATION_ASSIGNMENT ( #521, #5982, ( #3255 ) ) ;
#3674 = EDGE_LOOP ( 'NONE', ( #2573, #6610, #7316, #507 ) ) ;
#3675 = CYLINDRICAL_SURFACE ( 'NONE', #2189, 1.624999999999999778 ) ;
#3676 = CARTESIAN_POINT ( 'NONE',  ( -3.987046614173228587, 4.146499994074616779, 8.231249998505111520 ) ) ;
#3677 = LINE ( 'NONE', #5632, #4137 ) ;
#3678 = EDGE_LOOP ( 'NONE', ( #5613, #3138, #3134, #3447 ) ) ;
#3679 = COORDINATED_UNIVERSAL_TIME_OFFSET ( 0, 0, .AHEAD. ) ;
#3680 = CYLINDRICAL_SURFACE ( 'NONE', #5563, 0.3124999879509117728 ) ;
#3681 = DATE_AND_TIME ( #7442, #6419 ) ;
#3682 = ADVANCED_FACE ( 'NONE', ( #5963, #1086 ), #343, .T. ) ;
#3683 = CARTESIAN_POINT ( 'NONE',  ( -1.074999999999999289, 3.950000000000000178, -4.043750000000001066 ) ) ;
#3684 = FACE_OUTER_BOUND ( 'NONE', #6309, .T. ) ;
#3685 = CYLINDRICAL_SURFACE ( 'NONE', #1217, 0.4312500000000004663 ) ;
#3686 = ORIENTED_EDGE ( 'NONE', *, *, #3104, .F. ) ;
#3687 = CARTESIAN_POINT ( 'NONE',  ( -0.7491228847736894902, 3.991630787898853949, 8.541661844804179893 ) ) ;
#3688 = LENGTH_MEASURE_WITH_UNIT ( LENGTH_MEASURE( 0.02539999999999999897 ), #4380 );
#3689 = DIRECTION ( 'NONE',  ( -0.000000000000000000, 1.000000000000000000, -0.000000000000000000 ) ) ;
#3690 = PERSON_AND_ORGANIZATION ( #7862, #8117 ) ;
#3691 = EDGE_LOOP ( 'NONE', ( #4923, #7452, #5215, #6753 ) ) ;
#3692 = DIRECTION ( 'NONE',  ( 0.000000000000000000, 0.000000000000000000, 1.000000000000000000 ) ) ;
#3693 = EDGE_LOOP ( 'NONE', ( #7436, #3197, #8152, #4417, #4117, #573 ) ) ;
#3694 = FACE_OUTER_BOUND ( 'NONE', #3315, .T. ) ;
#3695 = FACE_BOUND ( 'NONE', #8103, .T. ) ;
#3696 = EDGE_CURVE ( 'NONE', #4281, #4445, #2965, .T. ) ;
#3697 = ORIENTED_EDGE ( 'NONE', *, *, #3163, .F. ) ;
#3698 = ORIENTED_EDGE ( 'NONE', *, *, #1192, .F. ) ;
#3699 = LOCAL_TIME ( 0, 37, 23.00000000000000000, #4736 ) ;
#3700 = CARTESIAN_POINT ( 'NONE',  ( 3.179822820131703587, 2.000074507168632554, -0.5625000000000001110 ) ) ;
#3701 = CARTESIAN_POINT ( 'NONE',  ( 2.750000000000000000, 7.521783346412262539, 3.956250000092213615 ) ) ;
#3702 = CARTESIAN_POINT ( 'NONE',  ( 1.187500000000000000, 4.527538552213043133, 6.353289427497075259 ) ) ;
#3703 = VERTEX_POINT ( 'NONE', #8021 ) ;
#3704 = APPROVAL_STATUS ( 'not_yet_approved' ) ;
#3705 = CARTESIAN_POINT ( 'NONE',  ( -2.750000000000000444, 8.719000000000002970, 3.823750000000002647 ) ) ;
#3706 = VECTOR ( 'NONE', #4624, 39.37007874015748143 ) ;
#3707 = LOCAL_TIME ( 0, 37, 23.00000000000000000, #5503 ) ;
#3708 = EDGE_CURVE ( 'NONE', #3004, #2473, #2358, .T. ) ;
#3709 = VECTOR ( 'NONE', #1011, 39.37007874015748143 ) ;
#3710 = CIRCLE ( 'NONE', #176, 0.2625000000000008438 ) ;
#3711 = LOCAL_TIME ( 0, 37, 23.00000000000000000, #1531 ) ;
#3712 = FACE_OUTER_BOUND ( 'NONE', #7836, .T. ) ;
#3713 = ORIENTED_EDGE ( 'NONE', *, *, #7424, .F. ) ;
#3714 = COORDINATED_UNIVERSAL_TIME_OFFSET ( 0, 0, .AHEAD. ) ;
#3715 = CARTESIAN_POINT ( 'NONE',  ( -2.750000000000000444, 8.729000000000002757, 3.333750000000001990 ) ) ;
#3716 = ITEM_DEFINED_TRANSFORMATION ( 'NONE', 'NONE', #4248,  #7272 ) ;
#3717 = CC_DESIGN_PERSON_AND_ORGANIZATION_ASSIGNMENT ( #5239, #6540, ( #6746 ) ) ;
#3718 = PLANE ( 'NONE',  #5315 ) ;
#3719 = CIRCLE ( 'NONE', #5414, 0.4312500000000004663 ) ;
#3720 = CARTESIAN_POINT ( 'NONE',  ( -3.987046614173228587, 3.755224612465394518, 8.200350840132131225 ) ) ;
#3721 = DIRECTION ( 'NONE',  ( 0.000000000000000000, 0.000000000000000000, 1.000000000000000000 ) ) ;
#3722 = DIRECTION ( 'NONE',  ( 1.000000000000000000, 0.000000000000000000, 0.000000000000000000 ) ) ;
#3723 = EDGE_LOOP ( 'NONE', ( #4141, #3662 ) ) ;
#3724 = CARTESIAN_POINT ( 'NONE',  ( -0.6829499219002715948, 4.259968811991060811, 8.272284810380442721 ) ) ;
#3725 = VECTOR ( 'NONE', #7805, 39.37007874015748143 ) ;
#3726 = CARTESIAN_POINT ( 'NONE',  ( -1.054418134971605747, 4.854198021652829098, 6.858307716535429144 ) ) ;
#3727 = AXIS2_PLACEMENT_3D ( 'NONE', #3801, #568, #7531 ) ;
#3728 = APPROVAL_ROLE ( '' ) ;
#3729 = ORIENTED_EDGE ( 'NONE', *, *, #4762, .F. ) ;
#3730 = CARTESIAN_POINT ( 'NONE',  ( 0.000000000000000000, 3.950000000000000178, 6.956250000000000711 ) ) ;
#3731 = B_SPLINE_CURVE_WITH_KNOTS ( 'NONE', 3,
 ( #8168, #5637, #139, #99, #4451, #1340 ),
 .UNSPECIFIED., .F., .F.,
 ( 4, 2, 4 ),
 ( 2.166691104215167967E-12, 0.007631658729071641098, 0.01526331745597659002 ),
 .UNSPECIFIED. ) ;
#3732 = EDGE_CURVE ( 'NONE', #2439, #3378, #7107, .T. ) ;
#3733 = ORIENTED_EDGE ( 'NONE', *, *, #670, .F. ) ;
#3734 = DIRECTION ( 'NONE',  ( 0.000000000000000000, 0.000000000000000000, 1.000000000000000000 ) ) ;
#3735 = EDGE_CURVE ( 'NONE', #2229, #6048, #5271, .T. ) ;
#3736 = CARTESIAN_POINT ( 'NONE',  ( 0.000000000000000000, 0.000000000000000000, 0.000000000000000000 ) ) ;
#3737 = VECTOR ( 'NONE', #4433, 39.37007874015748143 ) ;
#3738 = EDGE_LOOP ( 'NONE', ( #1783, #4605, #1029, #1413 ) ) ;
#3739 = EDGE_CURVE ( 'NONE', #2476, #6635, #7376, .T. ) ;
#3740 = EDGE_LOOP ( 'NONE', ( #4543, #2063, #2761, #3782 ) ) ;
#3741 = CARTESIAN_POINT ( 'NONE',  ( 2.946793809113656959, 2.499999999120089189, 0.5624999991014997258 ) ) ;
#3742 = CARTESIAN_POINT ( 'NONE',  ( 0.08551594028232864519, 2.637422184226597022, -5.108750000000001457 ) ) ;
#3743 = CARTESIAN_POINT ( 'NONE',  ( 1.187500000000000222, 4.620056610596821933, 6.126062285476682412 ) ) ;
#3744 = EDGE_LOOP ( 'NONE', ( #7307, #1649, #1736, #5867 ) ) ;
#3745 = CALENDAR_DATE ( 2026, 8, 10 ) ;
#3746 = CARTESIAN_POINT ( 'NONE',  ( -2.740000000000001545, 8.719000000000002970, 4.323750000000001315 ) ) ;
#3747 = AXIS2_PLACEMENT_3D ( 'NONE', #3149, #6800, #3114 ) ;
#3748 = ORIENTED_EDGE ( 'NONE', *, *, #2086, .F. ) ;
#3749 = EDGE_CURVE ( 'NONE', #4674, #1923, #3452, .T. ) ;
#3750 = ORIENTED_EDGE ( 'NONE', *, *, #388, .T. ) ;
#3751 = AXIS2_PLACEMENT_3D ( 'NONE', #5424, #7986, #2326 ) ;
#3752 = VECTOR ( 'NONE', #3218, 39.37007874015748143 ) ;
#3753 = CARTESIAN_POINT ( 'NONE',  ( 0.000000000000000000, 7.964000000000000412, 0.000000000000000000 ) ) ;
#3754 = CARTESIAN_POINT ( 'NONE',  ( -2.750000000000000444, 7.521783346446679452, 3.691250000461920422 ) ) ;
#3755 = DIRECTION ( 'NONE',  ( -1.000000000000000000, 0.000000000000000000, 0.000000000000000000 ) ) ;
#3756 = ORIENTED_EDGE ( 'NONE', *, *, #830, .F. ) ;
#3757 = DATE_AND_TIME ( #4982, #5260 ) ;
#3758 = FACE_OUTER_BOUND ( 'NONE', #1390, .T. ) ;
#3759 = APPROVAL_STATUS ( 'not_yet_approved' ) ;
#3760 = DIRECTION ( 'NONE',  ( 0.7071067811865474617, 0.000000000000000000, -0.7071067811865474617 ) ) ;
#3761 = FACE_OUTER_BOUND ( 'NONE', #1313, .T. ) ;
#3762 = DIMENSIONAL_EXPONENTS ( 1.000000000000000000, 0.000000000000000000, 0.000000000000000000, 0.000000000000000000, 0.000000000000000000, 0.000000000000000000, 0.000000000000000000 ) ;
#3763 = CARTESIAN_POINT ( 'NONE',  ( -3.987046614173229475, 3.766169374065349906, 8.161828647665473113 ) ) ;
#3764 = CC_DESIGN_DATE_AND_TIME_ASSIGNMENT ( #7640, #683, ( #4775 ) ) ;
#3765 = CARTESIAN_POINT ( 'NONE',  ( 0.000000000000000000, 5.145404907950669404, 6.923631455418962410 ) ) ;
#3766 = ORIENTED_EDGE ( 'NONE', *, *, #2585, .T. ) ;
#3767 = CARTESIAN_POINT ( 'NONE',  ( -2.750000000000000444, 7.339000000000001300, 4.486250000000000959 ) ) ;
#3768 = CARTESIAN_POINT ( 'NONE',  ( 2.750000000000000444, 8.729000000000002757, 3.823750000000002647 ) ) ;
#3769 = CARTESIAN_POINT ( 'NONE',  ( 3.182000000000000828, 5.541000000000003922, 3.956250000000000266 ) ) ;
#3770 = APPROVAL_DATE_TIME ( #7653, #5165 ) ;
#3771 = CC_DESIGN_SECURITY_CLASSIFICATION ( #4146, ( #8153 ) ) ;
#3772 = ORIENTED_EDGE ( 'NONE', *, *, #1810, .T. ) ;
#3773 = PLANE ( 'NONE',  #8007 ) ;
#3774 = FACE_OUTER_BOUND ( 'NONE', #4202, .T. ) ;
#3775 = DIRECTION ( 'NONE',  ( 0.000000000000000000, 0.000000000000000000, 1.000000000000000000 ) ) ;
#3776 = ORIENTED_EDGE ( 'NONE', *, *, #8030, .F. ) ;
#3777 = ORIENTED_EDGE ( 'NONE', *, *, #224, .F. ) ;
#3778 = EDGE_CURVE ( 'NONE', #4596, #6749, #8093, .T. ) ;
#3779 = CARTESIAN_POINT ( 'NONE',  ( 3.987953385826771058, 4.144775419411346640, 8.200350840128573182 ) ) ;
#3780 = CARTESIAN_POINT ( 'NONE',  ( 1.291725143358333661, 4.183586393851094876, -5.108749999999998792 ) ) ;
#3781 = CARTESIAN_POINT ( 'NONE',  ( 1.187500000000001110, 4.349209729547924397, 6.675164255166571081 ) ) ;
#3782 = ORIENTED_EDGE ( 'NONE', *, *, #1581, .F. ) ;
#3783 = DATE_AND_TIME ( #2453, #7409 ) ;
#3784 = CARTESIAN_POINT ( 'NONE',  ( 0.000000000000000000, 5.339000000000000412, 0.1249999999999997641 ) ) ;
#3785 = VERTEX_POINT ( 'NONE', #3741 ) ;
#3786 = DIRECTION ( 'NONE',  ( 0.000000000000000000, -0.000000000000000000, 1.000000000000000000 ) ) ;
#3787 = DIRECTION ( 'NONE',  ( -1.000000000000000000, -0.000000000000000000, 0.000000000000000000 ) ) ;
#3788 = CARTESIAN_POINT ( 'NONE',  ( 2.577468385826771957, 5.238734212598424200, 3.956250000000000266 ) ) ;
#3789 = EDGE_LOOP ( 'NONE', ( #5204, #6885, #2651, #2728 ) ) ;
#3790 = DATE_TIME_ROLE ( 'creation_date' ) ;
#3791 = CARTESIAN_POINT ( 'NONE',  ( 3.987953385826772390, 3.950000015938371689, 7.918750010554200358 ) ) ;
#3792 = ITEM_DEFINED_TRANSFORMATION ( 'NONE', 'NONE', #1249,  #7272 ) ;
#3793 = CARTESIAN_POINT ( 'NONE',  ( -2.740000000000000657, 7.964000000000000412, 3.823750000000002647 ) ) ;
#3794 = CARTESIAN_POINT ( 'NONE',  ( -8.751021560936518753E-10, 1.000000000000000222, 5.750408897959578548E-10 ) ) ;
#3795 = LOCAL_TIME ( 0, 37, 23.00000000000000000, #2905 ) ;
#3796 = CARTESIAN_POINT ( 'NONE',  ( -3.987046614173229475, 3.836846444618186691, 8.070563664178971308 ) ) ;
#3797 = DIRECTION ( 'NONE',  ( 0.000000000000000000, 0.000000000000000000, -1.000000000000000000 ) ) ;
#3798 = DIRECTION ( 'NONE',  ( 0.000000000000000000, 0.000000000000000000, -1.000000000000000000 ) ) ;
#3799 = EDGE_LOOP ( 'NONE', ( #5384, #1847, #2123 ) ) ;
#3800 = CARTESIAN_POINT ( 'NONE',  ( -2.750000000000000444, 7.964000000000000412, 5.236250000000000071 ) ) ;
#3801 = CARTESIAN_POINT ( 'NONE',  ( 0.000000000000000000, 0.000000000000000000, 0.000000000000000000 ) ) ;
#3802 = DIRECTION ( 'NONE',  ( 1.000000000000000000, 0.000000000000000000, 0.000000000000000000 ) ) ;
#3803 = PERSON_AND_ORGANIZATION ( #7862, #8117 ) ;
#3804 = ORIENTED_EDGE ( 'NONE', *, *, #7832, .F. ) ;
#3805 = DIRECTION ( 'NONE',  ( -1.000000000000000000, 0.000000000000000000, 0.000000000000000000 ) ) ;
#3806 = DIMENSIONAL_EXPONENTS ( 1.000000000000000000, 0.000000000000000000, 0.000000000000000000, 0.000000000000000000, 0.000000000000000000, 0.000000000000000000, 0.000000000000000000 ) ;
#3807 = CARTESIAN_POINT ( 'NONE',  ( -2.740000000000000213, 8.729000000000002757, 3.333750000000001990 ) ) ;
#3808 = LINE ( 'NONE', #1320, #6345 ) ;
#3809 = DIRECTION ( 'NONE',  ( 0.7071067811865474617, 0.7071067811865474617, -0.000000000000000000 ) ) ;
#3810 = EDGE_LOOP ( 'NONE', ( #1395, #7962 ) ) ;
#3811 = ORIENTED_EDGE ( 'NONE', *, *, #78, .T. ) ;
#3812 = APPROVAL ( #4815, 'UNSPECIFIED' ) ;
#3813 = CARTESIAN_POINT ( 'NONE',  ( 3.987953385826772390, 3.806261876193907767, 8.097094170351185838 ) ) ;
#3814 = CARTESIAN_POINT ( 'NONE',  ( 0.4206575512004037121, 2.705990808344437948, -5.108749999999997904 ) ) ;
#3815 = FACE_OUTER_BOUND ( 'NONE', #1904, .T. ) ;
#3816 = ORIENTED_EDGE ( 'NONE', *, *, #7093, .F. ) ;
#3817 = CARTESIAN_POINT ( 'NONE',  ( -2.750000000000000444, 7.964000000000000412, 4.313750000000002416 ) ) ;
#3818 = ORIENTED_EDGE ( 'NONE', *, *, #2536, .T. ) ;
#3819 = EDGE_CURVE ( 'NONE', #3476, #5226, #7508, .T. ) ;
#3820 = EDGE_CURVE ( 'NONE', #2183, #7868, #6162, .T. ) ;
#3821 = CARTESIAN_POINT ( 'NONE',  ( -0.001186137648316157355, 2.637500537863615158, -5.108750000000001457 ) ) ;
#3822 = CARTESIAN_POINT ( 'NONE',  ( 2.577468385826771957, 2.661265787401575267, 3.956250000000000266 ) ) ;
#3823 = DIRECTION ( 'NONE',  ( 1.000000000000000000, 0.000000000000000000, 0.000000000000000000 ) ) ;
#3824 = EDGE_LOOP ( 'NONE', ( #1789, #5997, #6844, #5437 ) ) ;
#3825 = COORDINATED_UNIVERSAL_TIME_OFFSET ( 0, 0, .AHEAD. ) ;
#3826 = VECTOR ( 'NONE', #7566, 39.37007874015748143 ) ;
#3827 = FACE_OUTER_BOUND ( 'NONE', #1234, .T. ) ;
#3828 = CC_DESIGN_APPROVAL ( #1862, ( #7978 ) ) ;
#3829 = PERSON_AND_ORGANIZATION_ROLE ( 'classification_officer' ) ;
#3830 = CARTESIAN_POINT ( 'NONE',  ( -2.537500000000000533, 1.664000000000000368, 0.000000000000000000 ) ) ;
#3831 = PRODUCT_DEFINITION_SHAPE ( 'NONE', 'NONE',  #8191 ) ;
#3832 = CIRCLE ( 'NONE', #2273, 0.1875000000000006661 ) ;
#3833 = EDGE_CURVE ( 'NONE', #540, #7519, #4652, .T. ) ;
#3834 = DIRECTION ( 'NONE',  ( -0.000000000000000000, -1.000000000000000000, 0.000000000000000000 ) ) ;
#3835 = DIRECTION ( 'NONE',  ( 0.000000000000000000, -1.000000000000000000, 0.000000000000000000 ) ) ;
#3836 = EDGE_LOOP ( 'NONE', ( #3277, #458 ) ) ;
#3837 = CARTESIAN_POINT ( 'NONE',  ( 0.000000000000000000, 7.521783347225603045, 3.691250000923840258 ) ) ;
#3838 =( NAMED_UNIT ( * ) SI_UNIT ( $, .STERADIAN. ) SOLID_ANGLE_UNIT ( ) );
#3839 = CARTESIAN_POINT ( 'NONE',  ( -2.750000000000000444, 8.589000000000000412, 5.236250000000000071 ) ) ;
#3840 = DIRECTION ( 'NONE',  ( -0.7071067811865474617, 0.000000000000000000, -0.7071067811865474617 ) ) ;
#3841 = AXIS2_PLACEMENT_3D ( 'NONE', #2319, #5588, #4227 ) ;
#3842 = SECURITY_CLASSIFICATION_LEVEL ( 'unclassified' ) ;
#3843 = ORIENTED_EDGE ( 'NONE', *, *, #3778, .T. ) ;
#3844 = VECTOR ( 'NONE', #3434, 39.37007874015748143 ) ;
#3845 = DIRECTION ( 'NONE',  ( 0.000000000000000000, 0.000000000000000000, -1.000000000000000000 ) ) ;
#3846 = CIRCLE ( 'NONE', #7960, 2.619834133858267577 ) ;
#3847 = DIRECTION ( 'NONE',  ( 0.000000000000000000, 0.000000000000000000, 1.000000000000000000 ) ) ;
#3848 = DIRECTION ( 'NONE',  ( -0.000000000000000000, 1.000000000000000000, 0.000000000000000000 ) ) ;
#3849 = DIRECTION ( 'NONE',  ( 0.000000000000000000, 0.000000000000000000, -1.000000000000000000 ) ) ;
#3850 = ORIENTED_EDGE ( 'NONE', *, *, #2044, .T. ) ;
#3851 = AXIS2_PLACEMENT_3D ( 'NONE', #6572, #2246, #5312 ) ;
#3852 = ORIENTED_EDGE ( 'NONE', *, *, #1210, .F. ) ;
#3853 = AXIS2_PLACEMENT_3D ( 'NONE', #3193, #67, #4334 ) ;
#3854 = CARTESIAN_POINT ( 'NONE',  ( 3.987953385826774166, 3.781899934594699975, 8.129275075081856983 ) ) ;
#3855 = CONICAL_SURFACE ( 'NONE', #3483, 3.343750000098590913, 0.4297622790966889594 ) ;
#3856 = PRODUCT_DEFINITION ( 'UNKNOWN', '', #2206, #4800 ) ;
#3857 = CARTESIAN_POINT ( 'NONE',  ( 1.242854517407008030, 3.525957823492111398, -5.108750000000003233 ) ) ;
#3858 = APPROVAL_PERSON_ORGANIZATION ( #7063, #2421, #4398 ) ;
#3859 = LINE ( 'NONE', #1497, #6101 ) ;
#3860 = CARTESIAN_POINT ( 'NONE',  ( 3.987953385826772390, 3.766726267967030140, 8.302127249793056052 ) ) ;
#3861 = EDGE_LOOP ( 'NONE', ( #1968, #485 ) ) ;
#3862 = CIRCLE ( 'NONE', #1794, 0.3625000000000019318 ) ;
#3863 = DIRECTION ( 'NONE',  ( -0.000000000000000000, -0.000000000000000000, 1.000000000000000000 ) ) ;
#3864 = CARTESIAN_POINT ( 'NONE',  ( -1.625000000000000222, 5.113999999999999879, -2.750000000000000444 ) ) ;
#3865 = AXIS2_PLACEMENT_3D ( 'NONE', #564, #5640, #2541 ) ;
#3866 = ORIENTED_EDGE ( 'NONE', *, *, #2598, .F. ) ;
#3867 = PERSON_AND_ORGANIZATION ( #7862, #8117 ) ;
#3868 = DIRECTION ( 'NONE',  ( 0.000000000000000000, -0.000000000000000000, -1.000000000000000000 ) ) ;
#3869 = FACE_OUTER_BOUND ( 'NONE', #1755, .T. ) ;
#3870 = CARTESIAN_POINT ( 'NONE',  ( -0.7499999999999993339, 3.950000000000000178, 8.231250000000001066 ) ) ;
#3871 = VECTOR ( 'NONE', #523, 39.37007874015748143 ) ;
#3872 = EDGE_LOOP ( 'NONE', ( #8057, #629, #7174, #6077 ) ) ;
#3873 = CARTESIAN_POINT ( 'NONE',  ( 0.000000000000000000, 3.001975734461090560E-16, 0.000000000000000000 ) ) ;
#3874 = CARTESIAN_POINT ( 'NONE',  ( 2.513411990276540831, 1.000000000000000222, -2.949302488239232023 ) ) ;
#3875 = EDGE_CURVE ( 'NONE', #3252, #4495, #4225, .T. ) ;
#3876 = CARTESIAN_POINT ( 'NONE',  ( -3.987046614173229475, 4.133830657811391696, 8.300671349345057237 ) ) ;
#3877 = EDGE_LOOP ( 'NONE', ( #3661, #2195, #1554, #3143 ) ) ;
#3878 = CARTESIAN_POINT ( 'NONE',  ( -4.382879947506561180, 3.516000035344543306, 9.099249959692771839 ) ) ;
#3879 =( NAMED_UNIT ( * ) PLANE_ANGLE_UNIT ( ) SI_UNIT ( $, .RADIAN. ) );
#3880 = CARTESIAN_POINT ( 'NONE',  ( -1.187500000000000000, 4.662394452531453126, 6.009229019005898564 ) ) ;
#3881 = PERSON_AND_ORGANIZATION ( #7862, #8117 ) ;
#3882 = VERTEX_POINT ( 'NONE', #6818 ) ;
#3883 = CARTESIAN_POINT ( 'NONE',  ( 1.624999999999999778, 3.950000000000000178, -5.108750000000001457 ) ) ;
#3884 = DIRECTION ( 'NONE',  ( -1.000000000000000000, 0.000000000000000000, 0.000000000000000000 ) ) ;
#3885 = EDGE_LOOP ( 'NONE', ( #5907, #4272, #3467, #1657, #1514, #1048, #7501, #3913 ) ) ;
#3886 = CARTESIAN_POINT ( 'NONE',  ( -0.7457411423250316362, 3.867608449240891311, 7.929090657501175698 ) ) ;
#3887 = VERTEX_POINT ( 'NONE', #541 ) ;
#3888 = EDGE_CURVE ( 'NONE', #47, #7868, #5622, .T. ) ;
#3889 = UNCERTAINTY_MEASURE_WITH_UNIT (LENGTH_MEASURE( 1.000000000000000082E-05 ), #908, 'distance_accuracy_value', 'NONE');
#3890 = LOCAL_TIME ( 0, 37, 23.00000000000000000, #2666 ) ;
#3891 = CARTESIAN_POINT ( 'NONE',  ( -0.6000000000000015321, 3.950000000000000178, 8.981250000000001066 ) ) ;
#3892 = CARTESIAN_POINT ( 'NONE',  ( 1.312565956928763322, 3.990720461577614842, -5.108749999999999680 ) ) ;
#3893 = LOCAL_TIME ( 0, 37, 23.00000000000000000, #5313 ) ;
#3894 = PLANE ( 'NONE',  #5055 ) ;
#3895 = EDGE_LOOP ( 'NONE', ( #2616, #5784 ) ) ;
#3896 = PRODUCT ( 'bench vise6_3-', 'bench vise6_3-', '', ( #4972 ) ) ;
#3897 = CARTESIAN_POINT ( 'NONE',  ( 2.750000000000000888, 8.719000000000001194, 3.813750000000002416 ) ) ;
#3898 = FACE_OUTER_BOUND ( 'NONE', #4438, .T. ) ;
#3899 = VERTEX_POINT ( 'NONE', #1289 ) ;
#3900 = COORDINATED_UNIVERSAL_TIME_OFFSET ( 0, 0, .AHEAD. ) ;
#3901 = CARTESIAN_POINT ( 'NONE',  ( 4.462953385826772923, 4.146499994074616779, 8.624249954777599925 ) ) ;
#3902 = PERSON_AND_ORGANIZATION ( #5354, #2104 ) ;
#3903 = CARTESIAN_POINT ( 'NONE',  ( 0.6956352003900579950, 3.669529528902299997, 8.091948598562707318 ) ) ;
#3904 = CARTESIAN_POINT ( 'NONE',  ( -1.274606804493992884, 2.434036455850696168, -2.750000000000000444 ) ) ;
#3905 = CARTESIAN_POINT ( 'NONE',  ( 2.750000000000000888, 7.964000000000000412, 3.813750000000002416 ) ) ;
#3906 = PRODUCT_RELATED_PRODUCT_CATEGORY ( 'detail', '', ( #4564 ) ) ;
#3907 = VERTEX_POINT ( 'NONE', #4967 ) ;
#3908 = CARTESIAN_POINT ( 'NONE',  ( -3.987046614173227699, 3.980893307323864150, 8.036472273046369352 ) ) ;
#3909 = DIRECTION ( 'NONE',  ( -1.000000000000000000, -0.000000000000000000, 0.000000000000000000 ) ) ;
#3910 = CARTESIAN_POINT ( 'NONE',  ( -3.987046614173228587, 3.764952780856046122, 8.297661934734193778 ) ) ;
#3911 = ORIENTED_EDGE ( 'NONE', *, *, #7898, .T. ) ;
#3912 = DIRECTION ( 'NONE',  ( -7.142086257945775577E-16, -1.000000000000000000, 0.000000000000000000 ) ) ;
#3913 = ORIENTED_EDGE ( 'NONE', *, *, #4152, .F. ) ;
#3914 = DIRECTION ( 'NONE',  ( 0.0005594472316432074627, -8.255639090667793579E-17, 0.9999998435093854221 ) ) ;
#3915 = CARTESIAN_POINT ( 'NONE',  ( -2.750000000000000444, 7.339000000000003077, 5.236250000000000071 ) ) ;
#3916 = PLANE ( 'NONE',  #354 ) ;
#3917 = EDGE_CURVE ( 'NONE', #5506, #6895, #947, .T. ) ;
#3918 = DATE_AND_TIME ( #1561, #893 ) ;
#3919 =( BOUNDED_CURVE ( )  B_SPLINE_CURVE ( 2, ( #5760, #678, #3174, #7517, #6867, #3141, #2494 ),
 .UNSPECIFIED., .F., .T. ) 
 B_SPLINE_CURVE_WITH_KNOTS ( ( 3, 2, 2, 3 ),
 ( 0.000000000000000000, 0.01898937877529951676, 0.04622957262199210021, 0.05624330787783118901 ),
 .UNSPECIFIED. ) 
 CURVE ( )  GEOMETRIC_REPRESENTATION_ITEM ( )  RATIONAL_B_SPLINE_CURVE ( ( 0.8763122938253293803, 0.7958215604460294745, 1.000000000000000000, 0.7071067811865479058, 1.000000000000000000, 0.8923298722492541968, 0.8638207196608972405 ) ) 
 REPRESENTATION_ITEM ( '' )  );
#3920 = ORIENTED_EDGE ( 'NONE', *, *, #5708, .T. ) ;
#3921 = EDGE_CURVE ( 'NONE', #5733, #277, #3710, .T. ) ;
#3922 = CARTESIAN_POINT ( 'NONE',  ( -0.7499999999999993339, 3.950000000000000178, 7.918749999999998401 ) ) ;
#3923 = DIRECTION ( 'NONE',  ( 0.000000000000000000, 1.000000000000000000, 0.000000000000000000 ) ) ;
#3924 = CALENDAR_DATE ( 2026, 8, 10 ) ;
#3925 = ORIENTED_EDGE ( 'NONE', *, *, #6520, .F. ) ;
#3926 = CARTESIAN_POINT ( 'NONE',  ( -0.7432847975395561191, 3.848073801202759103, 7.935140446388324165 ) ) ;
#3927 = VERTEX_POINT ( 'NONE', #2639 ) ;
#3928 = CARTESIAN_POINT ( 'NONE',  ( 3.987953385826772834, 4.023056220426754592, 8.048833963766313104 ) ) ;
#3929 = EDGE_CURVE ( 'NONE', #5062, #2186, #2681, .T. ) ;
#3930 = CARTESIAN_POINT ( 'NONE',  ( -3.362500000000002931, 1.750000000000000000, -6.725000000000002309 ) ) ;
#3931 = FACE_OUTER_BOUND ( 'NONE', #3510, .T. ) ;
#3932 = CARTESIAN_POINT ( 'NONE',  ( 3.987953385826772390, 4.138119654530761693, 8.288651076799524731 ) ) ;
#3933 = ORIENTED_EDGE ( 'NONE', *, *, #3996, .F. ) ;
#3934 = DIRECTION ( 'NONE',  ( 0.000000000000000000, -1.000000000000000000, 0.000000000000000000 ) ) ;
#3935 = FACE_OUTER_BOUND ( 'NONE', #1308, .T. ) ;
#3936 = ORIENTED_EDGE ( 'NONE', *, *, #237, .F. ) ;
#3937 = COORDINATED_UNIVERSAL_TIME_OFFSET ( 0, 0, .AHEAD. ) ;
#3938 = CYLINDRICAL_SURFACE ( 'NONE', #728, 0.3625000012227142521 ) ;
#3939 = DATE_TIME_ROLE ( 'classification_date' ) ;
#3940 = CARTESIAN_POINT ( 'NONE',  ( 0.6994737761126067488, 3.679106805816449555, 8.074121781180350510 ) ) ;
#3941 = CARTESIAN_POINT ( 'NONE',  ( -1.198957880828181333, 2.500000000000000000, -2.750000000000000444 ) ) ;
#3942 = ORIENTED_EDGE ( 'NONE', *, *, #2647, .T. ) ;
#3943 = CIRCLE ( 'NONE', #1488, 0.3625000012227142521 ) ;
#3944 = SECURITY_CLASSIFICATION ( '', '', #3484 ) ;
#3945 = CARTESIAN_POINT ( 'NONE',  ( -3.987046614173229919, 3.831130030895572691, 8.388305332348675591 ) ) ;
#3946 = ORIENTED_EDGE ( 'NONE', *, *, #3921, .F. ) ;
#3947 = CARTESIAN_POINT ( 'NONE',  ( 0.000000000000000000, 2.359000000000000874, 3.956250000000000266 ) ) ;
#3948 = VERTEX_POINT ( 'NONE', #3891 ) ;
#3949 = DIRECTION ( 'NONE',  ( -0.6838295180757016922, -0.7296417229374683178, 0.0003825665906713948618 ) ) ;
#3950 = PRODUCT_RELATED_PRODUCT_CATEGORY ( 'detail', '', ( #6746 ) ) ;
#3951 = CARTESIAN_POINT ( 'NONE',  ( -2.750000000000000444, 7.521783346456695440, 3.956250000000000266 ) ) ;
#3952 = SHAPE_DEFINITION_REPRESENTATION ( #5562, #7355 ) ;
#3953 = ORIENTED_EDGE ( 'NONE', *, *, #19, .T. ) ;
#3954 = AXIS2_PLACEMENT_3D ( 'NONE', #583, #462, #7464 ) ;
#3955 = AXIS2_PLACEMENT_3D ( 'NONE', #3873, #6388, #771 ) ;
#3956 = EDGE_CURVE ( 'NONE', #2452, #938, #5141, .T. ) ;
#3957 = CC_DESIGN_SECURITY_CLASSIFICATION ( #1882, ( #8195 ) ) ;
#3958 = CARTESIAN_POINT ( 'NONE',  ( -1.177243217050785162, 4.531893234618878274, -5.108749999999998792 ) ) ;
#3959 = VECTOR ( 'NONE', #1088, 39.37007874015748143 ) ;
#3960 = DIRECTION ( 'NONE',  ( -0.000000000000000000, -1.000000000000000000, -0.000000000000000000 ) ) ;
#3961 = VECTOR ( 'NONE', #7429, 39.37007874015748854 ) ;
#3962 =( BOUNDED_CURVE ( )  B_SPLINE_CURVE ( 3, ( #3115, #5607, #16, #2423 ),
 .UNSPECIFIED., .F., .F. ) 
 B_SPLINE_CURVE_WITH_KNOTS ( ( 4, 4 ),
 ( 0.000000000000000000, 0.09552853956270015989 ),
 .UNSPECIFIED. ) 
 CURVE ( )  GEOMETRIC_REPRESENTATION_ITEM ( )  RATIONAL_B_SPLINE_CURVE ( ( 0.5192122202261599817, 0.5593999942402725356, 0.6626358111613523949, 0.8289196709893995596 ) ) 
 REPRESENTATION_ITEM ( '' )  );
#3963 = PRODUCT_DEFINITION_SHAPE ( 'NONE', 'NONE',  #8196 ) ;
#3964 = VECTOR ( 'NONE', #7150, 39.37007874015748143 ) ;
#3965 =( NAMED_UNIT ( * ) PLANE_ANGLE_UNIT ( ) SI_UNIT ( $, .RADIAN. ) );
#3966 = CARTESIAN_POINT ( 'NONE',  ( 0.7335700393700786970, 2.500000000000000444, -0.5625000000000003331 ) ) ;
#3967 = CC_DESIGN_APPROVAL ( #6874, ( #1914 ) ) ;
#3968 = ORIENTED_EDGE ( 'NONE', *, *, #5516, .T. ) ;
#3969 = APPROVAL_DATE_TIME ( #6582, #5566 ) ;
#3970 = ORIENTED_EDGE ( 'NONE', *, *, #8011, .T. ) ;
#3971 = CARTESIAN_POINT ( 'NONE',  ( 0.6889980206436410182, 3.653596005017109682, 8.332369961285712279 ) ) ;
#3972 = EDGE_CURVE ( 'NONE', #8146, #7577, #5013, .T. ) ;
#3973 = CIRCLE ( 'NONE', #3198, 3.874999999025058539 ) ;
#3974 = EDGE_CURVE ( 'NONE', #3397, #1533, #6500, .T. ) ;
#3975 = CARTESIAN_POINT ( 'NONE',  ( 0.000000000000000000, 3.950000000000000178, -2.750000000000000444 ) ) ;
#3976 = CARTESIAN_POINT ( 'NONE',  ( 3.987953385826771946, 4.225666661560477877, 8.231249998505111520 ) ) ;
#3977 = EDGE_CURVE ( 'NONE', #8086, #3578, #7588, .T. ) ;
#3978 = ADVANCED_FACE ( 'NONE', ( #7922 ), #2225, .T. ) ;
#3979 = CARTESIAN_POINT ( 'NONE',  ( 1.187500000000000444, 7.436775081392277720, 4.083473622006301262 ) ) ;
#3980 = EDGE_LOOP ( 'NONE', ( #3205, #4065, #4777, #6270, #6034 ) ) ;
#3981 = DIRECTION ( 'NONE',  ( -0.000000000000000000, 1.000000000000000000, 0.000000000000000000 ) ) ;
#3982 = ORIENTED_EDGE ( 'NONE', *, *, #817, .F. ) ;
#3983 = ADVANCED_FACE ( 'NONE', ( #3414 ), #2142, .F. ) ;
#3984 = AXIS2_PLACEMENT_3D ( 'NONE', #7998, #5473, #3016 ) ;
#3985 = DIRECTION ( 'NONE',  ( -1.000000000000000000, -0.000000000000000000, 0.000000000000000000 ) ) ;
#3986 = LINE ( 'NONE', #2234, #5418 ) ;
#3987 = EDGE_LOOP ( 'NONE', ( #7128, #148, #4855, #6776 ) ) ;
#3988 = DATE_AND_TIME ( #1508, #6461 ) ;
#3989 = CARTESIAN_POINT ( 'NONE',  ( -1.625000000000000222, 5.339000000000000412, 0.1249999999999997641 ) ) ;
#3990 = VECTOR ( 'NONE', #310, 39.37007874015748143 ) ;
#3991 = APPROVAL_ROLE ( '' ) ;
#3992 = CARTESIAN_POINT ( 'NONE',  ( 0.7210672075785409252, 3.743534557078039615, 7.996449899345008383 ) ) ;
#3993 = AXIS2_PLACEMENT_3D ( 'NONE', #264, #756, #6370 ) ;
#3994 = CARTESIAN_POINT ( 'NONE',  ( 0.7122963468828452660, 4.185277942229626902, 8.437904003344623760 ) ) ;
#3995 = DIRECTION ( 'NONE',  ( 0.000000000000000000, 0.000000000000000000, 1.000000000000000000 ) ) ;
#3996 = EDGE_CURVE ( 'NONE', #1711, #5062, #1230, .T. ) ;
#3997 = ORIENTED_EDGE ( 'NONE', *, *, #3499, .T. ) ;
#3998 = AXIS2_PLACEMENT_3D ( 'NONE', #2121, #7647, #3797 ) ;
#3999 = FACE_OUTER_BOUND ( 'NONE', #6539, .T. ) ;
#4000 = CARTESIAN_POINT ( 'NONE',  ( -3.987046614173228587, 3.781899934595456259, 8.333224921929698326 ) ) ;
#4001 = ORIENTED_EDGE ( 'NONE', *, *, #2396, .F. ) ;
#4002 = PLANE ( 'NONE',  #4637 ) ;
#4003 = CARTESIAN_POINT ( 'NONE',  ( -2.391141319651246544, 8.869983740348052592, 8.707787472742055002 ) ) ;
#4004 = CARTESIAN_POINT ( 'NONE',  ( -8.751021560936518753E-10, 1.000000000000000222, 5.750408897959578548E-10 ) ) ;
#4005 = DIRECTION ( 'NONE',  ( 1.000000000000000000, 0.000000000000000000, -0.000000000000000000 ) ) ;
#4006 = PERSON_AND_ORGANIZATION ( #7862, #8117 ) ;
#4007 = ORIENTED_EDGE ( 'NONE', *, *, #7277, .F. ) ;
#4008 = CIRCLE ( 'NONE', #7582, 3.874999999025058539 ) ;
#4009 = PRODUCT_RELATED_PRODUCT_CATEGORY ( 'detail', '', ( #1774 ) ) ;
#4010 = CARTESIAN_POINT ( 'NONE',  ( -1.102289202651617339, 4.662797418998615662, -5.108749999999997904 ) ) ;
#4011 = DIRECTION ( 'NONE',  ( 0.000000000000000000, -0.000000000000000000, 1.000000000000000000 ) ) ;
#4012 = CARTESIAN_POINT ( 'NONE',  ( 2.875000000000000888, 0.000000000000000000, -2.975000000000000977 ) ) ;
#4013 = EDGE_CURVE ( 'NONE', #1080, #615, #6198, .T. ) ;
#4014 = ORIENTED_EDGE ( 'NONE', *, *, #4834, .T. ) ;
#4015 = DATE_AND_TIME ( #334, #2916 ) ;
#4016 = ORIENTED_EDGE ( 'NONE', *, *, #6238, .F. ) ;
#4017 = CARTESIAN_POINT ( 'NONE',  ( -0.7314405957411597159, 3.783958348137107297, 7.966316554334126998 ) ) ;
#4018 = CARTESIAN_POINT ( 'NONE',  ( 2.750000000000000444, 8.601289606299213020, 3.323749999933555355 ) ) ;
#4019 = CARTESIAN_POINT ( 'NONE',  ( 4.383786719160105427, 3.516000035344543306, 7.363250037317454755 ) ) ;
#4020 = PLANE ( 'NONE',  #211 ) ;
#4021 = CARTESIAN_POINT ( 'NONE',  ( 3.987953385826772390, 4.093738155681345248, 8.365405826661140409 ) ) ;
#4022 = CARTESIAN_POINT ( 'NONE',  ( -0.7210672075785413693, 3.743534557078041836, 8.466050100654991084 ) ) ;
#4023 = ORIENTED_EDGE ( 'NONE', *, *, #743, .F. ) ;
#4024 = LOCAL_TIME ( 0, 37, 23.00000000000000000, #2002 ) ;
#4025 = ADVANCED_FACE ( 'NONE', ( #4638 ), #4092, .F. ) ;
#4026 = CARTESIAN_POINT ( 'NONE',  ( -8.751021560936518753E-10, 1.365923996832131609E-16, 5.750408897959578548E-10 ) ) ;
#4027 = DIRECTION ( 'NONE',  ( 0.000000000000000000, 1.000000000000000000, 0.000000000000000000 ) ) ;
#4028 = ORIENTED_EDGE ( 'NONE', *, *, #6889, .F. ) ;
#4029 = SHAPE_DEFINITION_REPRESENTATION ( #3001, #3570 ) ;
#4030 = CARTESIAN_POINT ( 'NONE',  ( 1.625000000000000222, 0.000000000000000000, 0.1249999999999997641 ) ) ;
#4031 = COORDINATED_UNIVERSAL_TIME_OFFSET ( 0, 0, .AHEAD. ) ;
#4032 = DIRECTION ( 'NONE',  ( 0.000000000000000000, -1.000000000000000000, 0.000000000000000000 ) ) ;
#4033 = ORIENTED_EDGE ( 'NONE', *, *, #1523, .T. ) ;
#4034 = DIRECTION ( 'NONE',  ( 1.000000000000000000, 0.000000000000000000, 0.000000000000000000 ) ) ;
#4035 = CARTESIAN_POINT ( 'NONE',  ( -3.987046614173228587, 4.133008534184505756, 8.302809606439751633 ) ) ;
#4036 = ORIENTED_EDGE ( 'NONE', *, *, #7898, .F. ) ;
#4037 = DIRECTION ( 'NONE',  ( 1.000000000000000000, -0.000000000000000000, -0.000000000000000000 ) ) ;
#4038 = EDGE_CURVE ( 'NONE', #1162, #1366, #7730, .T. ) ;
#4039 = ORIENTED_EDGE ( 'NONE', *, *, #5942, .F. ) ;
#4040 = EDGE_CURVE ( 'NONE', #1998, #7338, #1002, .T. ) ;
#4041 = FACE_OUTER_BOUND ( 'NONE', #936, .T. ) ;
#4042 = COORDINATED_UNIVERSAL_TIME_OFFSET ( 0, 0, .AHEAD. ) ;
#4043 = ORIENTED_EDGE ( 'NONE', *, *, #5327, .F. ) ;
#4044 = CARTESIAN_POINT ( 'NONE',  ( -1.267418543289768884, 4.291720194162276236, -5.108750000000002345 ) ) ;
#4045 = CARTESIAN_POINT ( 'NONE',  ( -3.987046614173228587, 4.225666661560477877, 8.231249998505111520 ) ) ;
#4046 = CARTESIAN_POINT ( 'NONE',  ( 2.537500000000000533, 2.500000000000000444, -0.4312500000000004663 ) ) ;
#4047 = CARTESIAN_POINT ( 'NONE',  ( 1.625000000000000222, 5.639000000000001123, -2.750000000000000444 ) ) ;
#4048 = APPROVAL_ROLE ( '' ) ;
#4049 = EDGE_LOOP ( 'NONE', ( #7143, #2835, #7903, #6182 ) ) ;
#4050 = CARTESIAN_POINT ( 'NONE',  ( -0.7491228847736897123, 3.908369212101148626, 7.920838155195822239 ) ) ;
#4051 = UNCERTAINTY_MEASURE_WITH_UNIT (LENGTH_MEASURE( 1.000000000000000082E-05 ), #5826, 'distance_accuracy_value', 'NONE');
#4052 = EDGE_CURVE ( 'NONE', #2861, #2772, #3832, .T. ) ;
#4053 = APPROVAL_PERSON_ORGANIZATION ( #3024, #2517, #8009 ) ;
#4054 = LINE ( 'NONE', #914, #7954 ) ;
#4055 = CARTESIAN_POINT ( 'NONE',  ( 4.383786719160104539, 4.383999996532200072, 8.231249998505111520 ) ) ;
#4056 = ORGANIZATION ( 'NAUO-ORG7', 'UNSPECIFIED', 'UNSPECIFIED' ) ;
#4057 = PRODUCT_RELATED_PRODUCT_CATEGORY ( 'detail', '', ( #1432 ) ) ;
#4058 = CARTESIAN_POINT ( 'NONE',  ( 3.987953385826772390, 3.874591561940604834, 8.412706550472572431 ) ) ;
#4059 = ORIENTED_EDGE ( 'NONE', *, *, #1606, .F. ) ;
#4060 = CARTESIAN_POINT ( 'NONE',  ( -1.625000000000000222, 5.339000000000000412, 0.1250000000000000278 ) ) ;
#4061 = CARTESIAN_POINT ( 'NONE',  ( -3.987046614173229475, 4.112654374748236918, 8.120947403352236194 ) ) ;
#4062 = DIRECTION ( 'NONE',  ( 1.000000000000000000, 0.000000000000000000, 0.000000000000000000 ) ) ;
#4063 = DIRECTION ( 'NONE',  ( -1.000000000000000000, 0.000000000000000000, 0.000000000000000000 ) ) ;
#4064 = CARTESIAN_POINT ( 'NONE',  ( 2.750000000000000888, 7.964000000000000412, 3.813750000000002416 ) ) ;
#4065 = ORIENTED_EDGE ( 'NONE', *, *, #3330, .F. ) ;
#4066 = DATE_AND_TIME ( #7381, #5533 ) ;
#4067 = DIRECTION ( 'NONE',  ( -0.000000000000000000, 1.000000000000000000, -0.000000000000000000 ) ) ;
#4068 = CARTESIAN_POINT ( 'NONE',  ( 0.6955978521287335958, 4.230565908133124609, 8.092097759609568897 ) ) ;
#4069 = ORIENTED_EDGE ( 'NONE', *, *, #3875, .T. ) ;
#4070 = CARTESIAN_POINT ( 'NONE',  ( -2.852014645669292303, 2.523992677165354248, 5.972081456692913015 ) ) ;
#4071 = ORIENTED_EDGE ( 'NONE', *, *, #882, .T. ) ;
#4072 = FACE_OUTER_BOUND ( 'NONE', #3744, .T. ) ;
#4073 = ORIENTED_EDGE ( 'NONE', *, *, #2585, .F. ) ;
#4074 = APPROVAL_DATE_TIME ( #486, #4273 ) ;
#4075 = DIRECTION ( 'NONE',  ( -0.7071067811865474617, 0.000000000000000000, -0.7071067811865474617 ) ) ;
#4076 = DATE_AND_TIME ( #1522, #1042 ) ;
#4077 = EDGE_LOOP ( 'NONE', ( #1867, #6096 ) ) ;
#4078 = DIRECTION ( 'NONE',  ( -0.5773502691896257311, -0.5773502691896257311, -0.5773502691896257311 ) ) ;
#4079 = EDGE_CURVE ( 'NONE', #1059, #6055, #3572, .T. ) ;
#4080 = CC_DESIGN_APPROVAL ( #4273, ( #7291 ) ) ;
#4081 = CARTESIAN_POINT ( 'NONE',  ( -1.270916235774476322, 3.611191510761752710, -5.108749999999999680 ) ) ;
#4082 = CARTESIAN_POINT ( 'NONE',  ( 0.4460230445270007560, 2.387088541186376922, 3.019143986898724652 ) ) ;
#4083 = CARTESIAN_POINT ( 'NONE',  ( 2.750000000000000444, 7.964000000000000412, 3.323750000000001759 ) ) ;
#4084 = CARTESIAN_POINT ( 'NONE',  ( -3.762484563843162100, 1.281112611882646579, 4.607714677951853639E-16 ) ) ;
#4085 = VECTOR ( 'NONE', #1700, 39.37007874015748854 ) ;
#4086 = DATE_TIME_ROLE ( 'creation_date' ) ;
#4087 = ORIENTED_EDGE ( 'NONE', *, *, #601, .T. ) ;
#4088 = AXIS2_PLACEMENT_3D ( 'NONE', #1693, #2349, #3618 ) ;
#4089 = CARTESIAN_POINT ( 'NONE',  ( 2.875000000000000888, 1.000000000000000222, -2.975000000000000977 ) ) ;
#4090 = EDGE_CURVE ( 'NONE', #2711, #7113, #4054, .T. ) ;
#4091 = VECTOR ( 'NONE', #3372, 39.37007874015748854 ) ;
#4092 = PLANE ( 'NONE',  #4490 ) ;
#4093 = LINE ( 'NONE', #1003, #4887 ) ;
#4094 = FACE_OUTER_BOUND ( 'NONE', #545, .T. ) ;
#4095 = CARTESIAN_POINT ( 'NONE',  ( 2.750000000000000444, 7.973999999999999311, 3.823750000000002647 ) ) ;
#4096 = CARTESIAN_POINT ( 'NONE',  ( -0.6817881100752515300, 3.637486043182223572, 8.221358888732334336 ) ) ;
#4097 = AXIS2_PLACEMENT_3D ( 'NONE', #77, #6492, #1975 ) ;
#4098 = ORIENTED_EDGE ( 'NONE', *, *, #296, .F. ) ;
#4099 = VECTOR ( 'NONE', #2993, 39.37007874015748854 ) ;
#4100 = B_SPLINE_CURVE_WITH_KNOTS ( 'NONE', 3,
 ( #7443, #2116, #275, #5804 ),
 .UNSPECIFIED., .F., .F.,
 ( 4, 4 ),
 ( 0.000000000000000000, 1.000000000000000000 ),
 .UNSPECIFIED. ) ;
#4101 = CC_DESIGN_PERSON_AND_ORGANIZATION_ASSIGNMENT ( #4337, #3234, ( #7597 ) ) ;
#4102 = DIRECTION ( 'NONE',  ( -1.000000000000000000, 0.000000000000000000, -0.000000000000000000 ) ) ;
#4103 = CARTESIAN_POINT ( 'NONE',  ( -1.462953685981321916, 1.365923996832131609E-16, 3.588229579027113481 ) ) ;
#4104 = AXIS2_PLACEMENT_3D ( 'NONE', #2936, #3598, #6172 ) ;
#4105 = DIRECTION ( 'NONE',  ( 0.000000000000000000, 0.000000000000000000, 1.000000000000000000 ) ) ;
#4106 = PERSON_AND_ORGANIZATION_ROLE ( 'design_supplier' ) ;
#4107 = LINE ( 'NONE', #4188, #2438 ) ;
#4108 = CARTESIAN_POINT ( 'NONE',  ( 3.987953385826772390, 3.753500037802128375, 8.231249998505111520 ) ) ;
#4109 = EDGE_CURVE ( 'NONE', #402, #1477, #2190, .T. ) ;
#4110 = CARTESIAN_POINT ( 'NONE',  ( 0.7122575715994515777, 4.185397438661337510, 8.024726960321796554 ) ) ;
#4111 = AXIS2_PLACEMENT_3D ( 'NONE', #2726, #5213, #6378 ) ;
#4112 = B_SPLINE_CURVE_WITH_KNOTS ( 'NONE', 3,
 ( #5140, #5855, #3428, #5924, #7729, #1511, #7686, #5805, #2038, #2699, #2117, #4573, #4610, #3994, #3470, #5973, #3513, #6675, #7247, #4692, #7208, #394, #977, #6010, #7860, #4728, #1593, #352, #1630, #4068, #2853, #7899, #4110, #2889, #5380, #7937, #2275, #4772, #7303, #1670, #5299, #4150, #2816, #4574 ),
 .UNSPECIFIED., .F., .F.,
 ( 4, 2, 2, 2, 2, 2, 2, 2, 2, 2, 2, 2, 2, 2, 2, 2, 2, 2, 2, 2, 2, 4 ),
 ( 0.02509446659736457724, 0.02666229889018166543, 0.02744621503659023035, 0.02823013118299879526, 0.02979796347581595978, 0.03058187962222452122, 0.03136579576863308960, 0.03293362806145024718, 0.03450146035426740476, 0.03528537650067598008, 0.03606929264708456234, 0.03763712493990171298, 0.03842104108631023973, 0.03920495723271877342, 0.04077278952553576447, 0.04234062181835274857, 0.04390845411116973268, 0.04547628640398672373, 0.04626020255039523660, 0.04704411869680374947, 0.04861195098962078215, 0.05017978328243780789 ),
 .UNSPECIFIED. ) ;
#4113 = ORIENTED_EDGE ( 'NONE', *, *, #7197, .F. ) ;
#4114 = CARTESIAN_POINT ( 'NONE',  ( 2.968750000000001332, 2.500000000000000444, 0.000000000000000000 ) ) ;
#4115 = ORIENTED_EDGE ( 'NONE', *, *, #7725, .F. ) ;
#4116 = PLANE ( 'NONE',  #4899 ) ;
#4117 = ORIENTED_EDGE ( 'NONE', *, *, #6953, .F. ) ;
#4118 = AXIS2_PLACEMENT_3D ( 'NONE', #5311, #7312, #7997 ) ;
#4119 = PERSON_AND_ORGANIZATION_ROLE ( 'design_owner' ) ;
#4120 = CARTESIAN_POINT ( 'NONE',  ( -1.625000000000000222, 0.000000000000000000, 0.000000000000000000 ) ) ;
#4121 = ADVANCED_FACE ( 'NONE', ( #4677, #421 ), #7191, .T. ) ;
#4122 = COORDINATED_UNIVERSAL_TIME_OFFSET ( 0, 0, .AHEAD. ) ;
#4123 = ORIENTED_EDGE ( 'NONE', *, *, #7987, .F. ) ;
#4124 = CARTESIAN_POINT ( 'NONE',  ( -1.625000000000000222, 2.359134605239151750, 2.598586947464774255 ) ) ;
#4125 = EDGE_CURVE ( 'NONE', #584, #5712, #2141, .T. ) ;
#4126 = EDGE_CURVE ( 'NONE', #2528, #7021, #6694, .T. ) ;
#4127 = FACE_BOUND ( 'NONE', #5483, .T. ) ;
#4128 = DIRECTION ( 'NONE',  ( 0.000000000000000000, 0.000000000000000000, -1.000000000000000000 ) ) ;
#4129 = CARTESIAN_POINT ( 'NONE',  ( -1.388463899750249738E-31, 3.950000000000000178, 3.440250000000000696 ) ) ;
#4130 = PERSON_AND_ORGANIZATION_ROLE ( 'classification_officer' ) ;
#4131 = EDGE_CURVE ( 'NONE', #7817, #2711, #5953, .T. ) ;
#4132 = ORIENTED_EDGE ( 'NONE', *, *, #2807, .T. ) ;
#4133 = CARTESIAN_POINT ( 'NONE',  ( 0.000000000000000000, 5.339000000000000412, -2.750000000000000444 ) ) ;
#4134 = UNCERTAINTY_MEASURE_WITH_UNIT (LENGTH_MEASURE( 1.000000000000000082E-05 ), #3153, 'distance_accuracy_value', 'NONE');
#4135 = B_SPLINE_CURVE_WITH_KNOTS ( 'NONE', 3,
 ( #8037, #2523, #5474, #7392, #6250, #639, #5011, #4400, #46, #172, #3377, #4022, #6549, #1577, #6589, #4562, #7070, #8059, #1047, #4271, #8104, #2440, #4929, #4096, #7286, #5369, #7105, #4555, #3286, #7660, #7022, #5282, #7065, #1411, #7146, #4017, #4635, #7189, #1449, #3926, #3886, #4050, #823, #6542 ),
 .UNSPECIFIED., .F., .F.,
 ( 4, 2, 2, 2, 2, 2, 2, 2, 2, 2, 2, 2, 2, 2, 2, 2, 2, 2, 2, 2, 2, 4 ),
 ( 0.000000000000000000, 0.001568404162335257888, 0.002352606243502886833, 0.003136808324670516644, 0.004705212487005845656, 0.005489414568173528811, 0.006273616649341211098, 0.007842020811676602560, 0.009410424974011993154, 0.01019462705517968151, 0.01097882913634736814, 0.01254723329868273791, 0.01333143537985037944, 0.01411563746101802269, 0.01568404162335322594, 0.01725244578568842918, 0.01882084994802362896, 0.02038925411035882873, 0.02117345619152645811, 0.02195765827269408402, 0.02352606243502932890, 0.02509446659736457724 ),
 .UNSPECIFIED. ) ;
#4136 = CIRCLE ( 'NONE', #1279, 1.624999999999999778 ) ;
#4137 = VECTOR ( 'NONE', #6297, 39.37007874015748143 ) ;
#4138 = CARTESIAN_POINT ( 'NONE',  ( 2.750000000000000444, 7.973999999999999311, 3.823750000000002647 ) ) ;
#4139 = CARTESIAN_POINT ( 'NONE',  ( 1.187500000722723215, 5.969165905511811587, 6.858307716535433585 ) ) ;
#4140 = CARTESIAN_POINT ( 'NONE',  ( 2.750000000000000888, 7.964000000000000412, 3.333750000000001990 ) ) ;
#4141 = ORIENTED_EDGE ( 'NONE', *, *, #3371, .T. ) ;
#4142 = CARTESIAN_POINT ( 'NONE',  ( -2.750000000000000444, 7.964000000000000412, 4.323750000000003091 ) ) ;
#4143 = DIRECTION ( 'NONE',  ( -1.000000000000000000, 7.142086257945775577E-16, 0.000000000000000000 ) ) ;
#4144 = FACE_OUTER_BOUND ( 'NONE', #3519, .T. ) ;
#4145 = EDGE_LOOP ( 'NONE', ( #6493, #7351, #984, #65 ) ) ;
#4147 = CALENDAR_DATE ( 2026, 8, 10 ) ;
#4146 = SECURITY_CLASSIFICATION ( '', '', #2094 ) ;
#4148 = CARTESIAN_POINT ( 'NONE',  ( -3.362500000000001155, 1.750000000000000444, 4.117874862132976456E-16 ) ) ;
#4149 = PERSON_AND_ORGANIZATION ( #570, #1317 ) ;
#4150 = CARTESIAN_POINT ( 'NONE',  ( 0.7491228847736894902, 3.991630787898853949, 7.920838155195820462 ) ) ;
#4151 = CARTESIAN_POINT ( 'NONE',  ( 1.312500000000000444, 8.589000000000000412, 2.411250000000000782 ) ) ;
#4152 = EDGE_CURVE ( 'NONE', #5232, #5017, #6988, .T. ) ;
#4153 = ORIENTED_EDGE ( 'NONE', *, *, #1322, .F. ) ;
#4154 = DIRECTION ( 'NONE',  ( -0.000000000000000000, -1.000000000000000000, -0.000000000000000000 ) ) ;
#4155 = ORIENTED_EDGE ( 'NONE', *, *, #3242, .T. ) ;
#4156 = CARTESIAN_POINT ( 'NONE',  ( 3.562500000000000444, 1.000000000000000222, 3.337500000000003020 ) ) ;
#4157 = ORIENTED_EDGE ( 'NONE', *, *, #4079, .T. ) ;
#4158 = APPROVAL_STATUS ( 'not_yet_approved' ) ;
#4159 = CARTESIAN_POINT ( 'NONE',  ( 3.987953385826771946, 3.753500037802130596, 8.624249954777599925 ) ) ;
#4160 = CARTESIAN_POINT ( 'NONE',  ( 1.187500002638678165, 4.186788052716939212, 6.858307716535433585 ) ) ;
#4161 = ITEM_DEFINED_TRANSFORMATION ( 'NONE', 'NONE', #5561,  #7272 ) ;
#4162 = ADVANCED_BREP_SHAPE_REPRESENTATION ( '', ( #4616, #7272 ), #1120 ) ;
#4163 = ORIENTED_EDGE ( 'NONE', *, *, #5623, .T. ) ;
#4164 = APPROVAL ( #7120, 'UNSPECIFIED' ) ;
#4165 = DIRECTION ( 'NONE',  ( 0.7071067811865554553, 1.586444216266441231E-14, -0.7071067811865394681 ) ) ;
#4166 = CARTESIAN_POINT ( 'NONE',  ( -0.2278558862525867923, 2.340729989832576852, 3.064709232292516017 ) ) ;
#4167 = CARTESIAN_POINT ( 'NONE',  ( -0.7499999999999992228, 3.970895372960746350, 7.918749999999996625 ) ) ;
#4168 = EDGE_CURVE ( 'NONE', #1442, #6680, #3497, .T. ) ;
#4169 = SHAPE_REPRESENTATION_RELATIONSHIP ( 'NONE' , 'NONE' ,  #578, #7219 ) ;
#4170 = CARTESIAN_POINT ( 'NONE',  ( -3.583510604133039568, 1.543025754838326824, 7.167021208266081800 ) ) ;
#4171 = CALENDAR_DATE ( 2026, 8, 10 ) ;
#4172 = EDGE_LOOP ( 'NONE', ( #3430, #4475 ) ) ;
#4173 = ADVANCED_FACE ( 'NONE', ( #6191 ), #3030, .T. ) ;
#4174 = LINE ( 'NONE', #376, #5195 ) ;
#4175 = CARTESIAN_POINT ( 'NONE',  ( -1.187500000000000444, 4.186788071090408181, 6.858307717089314970 ) ) ;
#4176 = DIRECTION ( 'NONE',  ( 4.440892098507806374E-15, 0.000000000000000000, 1.000000000000000000 ) ) ;
#4177 = CARTESIAN_POINT ( 'NONE',  ( 3.362500000000000711, 1.750000000000000444, -4.117874862132976456E-16 ) ) ;
#4178 = CARTESIAN_POINT ( 'NONE',  ( 0.000000000000000000, 2.762500000000000178, 6.956250000000000711 ) ) ;
#4179 = VERTEX_POINT ( 'NONE', #1236 ) ;
#4180 = LINE ( 'NONE', #2914, #2404 ) ;
#4181 = EDGE_LOOP ( 'NONE', ( #1409, #7786, #7155, #3287 ) ) ;
#4182 = CC_DESIGN_SECURITY_CLASSIFICATION ( #267, ( #8188 ) ) ;
#4183 = EDGE_CURVE ( 'NONE', #212, #5362, #3621, .T. ) ;
#4184 = CARTESIAN_POINT ( 'NONE',  ( 2.740000000000000657, 8.719000000000001194, 3.323750000000001759 ) ) ;
#4185 = DIRECTION ( 'NONE',  ( -7.142086257945775577E-16, -1.000000000000000000, 0.000000000000000000 ) ) ;
#4186 = LINE ( 'NONE', #1087, #3172 ) ;
#4187 = DIRECTION ( 'NONE',  ( 0.000000000000000000, 0.000000000000000000, -1.000000000000000000 ) ) ;
#4188 = CARTESIAN_POINT ( 'NONE',  ( -4.470366334113919926, 1.365923996832131609E-16, 2.937534001674281914 ) ) ;
#4189 = ORIENTED_EDGE ( 'NONE', *, *, #4953, .F. ) ;
#4190 = MECHANICAL_CONTEXT ( 'NONE', #4821, 'mechanical' ) ;
#4191 = CARTESIAN_POINT ( 'NONE',  ( -8.751021560936518753E-10, 1.365923996832131609E-16, 5.750408897959578548E-10 ) ) ;
#4192 = FACE_OUTER_BOUND ( 'NONE', #7708, .T. ) ;
#4193 = EDGE_CURVE ( 'NONE', #7866, #7102, #2435, .T. ) ;
#4194 = ORIENTED_EDGE ( 'NONE', *, *, #1642, .T. ) ;
#4195 = CARTESIAN_POINT ( 'NONE',  ( 1.625000000000000222, 5.339000000000000412, -2.750000000000000444 ) ) ;
#4196 = CARTESIAN_POINT ( 'NONE',  ( 3.687499987877262519, 1.000000000000000222, 3.874999999790589289 ) ) ;
#4197 = EDGE_LOOP ( 'NONE', ( #2626, #5974 ) ) ;
#4198 = PERSON_AND_ORGANIZATION ( #7862, #8117 ) ;
#4199 = CARTESIAN_POINT ( 'NONE',  ( 3.987953385826771946, 4.146499994074616779, 8.624249954777599925 ) ) ;
#4200 = DIRECTION ( 'NONE',  ( 0.000000000000000000, 0.000000000000000000, 1.000000000000000000 ) ) ;
#4201 = CONTEXT_DEPENDENT_SHAPE_REPRESENTATION ( #6282, #175 ) ;
#4202 = EDGE_LOOP ( 'NONE', ( #4039, #5861, #2723, #3272, #2595, #7115, #4808, #1596 ) ) ;
#4203 = DIRECTION ( 'NONE',  ( 0.000000000000000000, 1.000000000000000000, -0.000000000000000000 ) ) ;
#4204 = CC_DESIGN_DATE_AND_TIME_ASSIGNMENT ( #7457, #1116, ( #3413 ) ) ;
#4205 = CARTESIAN_POINT ( 'NONE',  ( -0.6854931847115989241, 4.254309166866921288, 8.159427574546592510 ) ) ;
#4206 = CARTESIAN_POINT ( 'NONE',  ( -1.388463899750249738E-31, 3.950000000000000178, 3.440250000000000696 ) ) ;
#4207 = PERSON_AND_ORGANIZATION ( #7862, #8117 ) ;
#4208 = ORIENTED_EDGE ( 'NONE', *, *, #224, .T. ) ;
#4209 = CARTESIAN_POINT ( 'NONE',  ( 3.762484563843159435, 1.281112611882646579, -7.524969127686321535 ) ) ;
#4210 = EDGE_CURVE ( 'NONE', #2711, #212, #6812, .T. ) ;
#4211 = CARTESIAN_POINT ( 'NONE',  ( 0.7499999999999993339, 3.950000000000000178, 7.231250000000000178 ) ) ;
#4212 = AXIS2_PLACEMENT_3D ( 'NONE', #423, #2996, #7285 ) ;
#4213 = AXIS2_PLACEMENT_3D ( 'NONE', #2013, #4636, #3532 ) ;
#4214 = CARTESIAN_POINT ( 'NONE',  ( 2.749999999999999556, 8.589000000000000412, 4.404023385826772774 ) ) ;
#4215 = CARTESIAN_POINT ( 'NONE',  ( 2.852014645669292303, 2.523992677165354248, 5.972081456692913015 ) ) ;
#4216 = ORIENTED_EDGE ( 'NONE', *, *, #7472, .T. ) ;
#4217 = DIRECTION ( 'NONE',  ( 0.000000000000000000, 0.000000000000000000, 1.000000000000000000 ) ) ;
#4218 = EDGE_CURVE ( 'NONE', #417, #1507, #4843, .T. ) ;
#4219 = ORIENTED_EDGE ( 'NONE', *, *, #2684, .F. ) ;
#4220 = ADVANCED_FACE ( 'NONE', ( #2957 ), #7539, .F. ) ;
#4221 = ADVANCED_FACE ( 'NONE', ( #4878 ), #1283, .F. ) ;
#4222 = CIRCLE ( 'NONE', #6464, 0.1875000000000006661 ) ;
#4223 = AXIS2_PLACEMENT_3D ( 'NONE', #3975, #5709, #83 ) ;
#4224 = EDGE_CURVE ( 'NONE', #3882, #7586, #7367, .T. ) ;
#4225 = LINE ( 'NONE', #3131, #7407 ) ;
#4226 = CARTESIAN_POINT ( 'NONE',  ( -3.343750000000001776, 1.750000000000000444, -0.5625000000000003331 ) ) ;
#4227 = DIRECTION ( 'NONE',  ( 0.000000000000000000, 0.000000000000000000, -1.000000000000000000 ) ) ;
#4228 = CARTESIAN_POINT ( 'NONE',  ( -1.462953685906409840, 1.000000000000000222, 3.588229579118171308 ) ) ;
#4229 = SHAPE_REPRESENTATION ( 'bench vise3-', ( #7272 ), #2017 ) ;
#4230 = ORIENTED_EDGE ( 'NONE', *, *, #5558, .T. ) ;
#4231 = SECURITY_CLASSIFICATION_LEVEL ( 'unclassified' ) ;
#4232 = VECTOR ( 'NONE', #4743, 39.37007874015748143 ) ;
#4233 = CARTESIAN_POINT ( 'NONE',  ( -1.500000000000000444, 5.339000000000000412, 0.1249999999999999445 ) ) ;
#4234 = AXIS2_PLACEMENT_3D ( 'NONE', #4567, #972, #4647 ) ;
#4235 = EDGE_CURVE ( 'NONE', #3703, #5265, #8147, .T. ) ;
#4236 = ORIENTED_EDGE ( 'NONE', *, *, #4842, .F. ) ;
#4237 = VECTOR ( 'NONE', #5650, 39.37007874015748143 ) ;
#4238 = DIRECTION ( 'NONE',  ( -0.000000000000000000, -1.000000000000000000, -0.000000000000000000 ) ) ;
#4239 = CARTESIAN_POINT ( 'NONE',  ( 0.000000000000000000, 3.950000000000000178, 8.831250000000000711 ) ) ;
#4240 = CARTESIAN_POINT ( 'NONE',  ( 3.651126734928074491, 1.365923996832131609E-16, -1.298036420927624057 ) ) ;
#4241 = ORIENTED_EDGE ( 'NONE', *, *, #3382, .F. ) ;
#4242 = DATE_AND_TIME ( #5389, #5527 ) ;
#4243 = DIRECTION ( 'NONE',  ( 0.000000000000000000, 0.000000000000000000, -1.000000000000000000 ) ) ;
#4244 = CIRCLE ( 'NONE', #2683, 2.999999999940156759 ) ;
#4245 = CARTESIAN_POINT ( 'NONE',  ( -0.4616491105740681000, 5.179384528936357590, -5.108750000000002345 ) ) ;
#4246 = PERSON_AND_ORGANIZATION_ROLE ( 'classification_officer' ) ;
#4247 = EDGE_CURVE ( 'NONE', #539, #3034, #3719, .T. ) ;
#4248 = AXIS2_PLACEMENT_3D ( 'NONE', #4544, #6435, #7054 ) ;
#4249 = PRODUCT_DEFINITION_SHAPE ( 'NONE', 'NONE',  #3856 ) ;
#4250 = EDGE_CURVE ( 'NONE', #5456, #2112, #1195, .T. ) ;
#4251 = VECTOR ( 'NONE', #3345, 39.37007874015748143 ) ;
#4252 = LINE ( 'NONE', #6879, #2455 ) ;
#4253 = VERTEX_POINT ( 'NONE', #461 ) ;
#4254 = CARTESIAN_POINT ( 'NONE',  ( -4.462046614173229564, 4.146499994074616779, 8.231249998505111520 ) ) ;
#4255 = SHAPE_REPRESENTATION_RELATIONSHIP ( 'NONE' , 'NONE' ,  #5548, #6817 ) ;
#4256 = CARTESIAN_POINT ( 'NONE',  ( -1.187500000000000444, 4.186788071090408181, 6.858307717089314970 ) ) ;
#4257 = CARTESIAN_POINT ( 'NONE',  ( -1.625000000000000222, 2.057992047244095346, -2.750000000000000444 ) ) ;
#4258 = PERSON_AND_ORGANIZATION ( #7862, #8117 ) ;
#4259 = ORIENTED_EDGE ( 'NONE', *, *, #1876, .F. ) ;
#4260 = CARTESIAN_POINT ( 'NONE',  ( -3.762484563843162100, 1.281112611882646579, 4.607714677951853639E-16 ) ) ;
#4261 = CIRCLE ( 'NONE', #2176, 0.3625000012227142521 ) ;
#4262 = CC_DESIGN_PERSON_AND_ORGANIZATION_ASSIGNMENT ( #1603, #6532, ( #3381 ) ) ;
#4263 = ORIENTED_EDGE ( 'NONE', *, *, #1386, .F. ) ;
#4264 = VECTOR ( 'NONE', #2974, 39.37007874015748143 ) ;
#4265 = EDGE_CURVE ( 'NONE', #4344, #7866, #1776, .T. ) ;
#4266 = DIRECTION ( 'NONE',  ( 0.000000000000000000, 0.000000000000000000, -1.000000000000000000 ) ) ;
#4267 = AXIS2_PLACEMENT_3D ( 'NONE', #7158, #1583, #4062 ) ;
#4268 = DIRECTION ( 'NONE',  ( -1.000000000000000000, 0.000000000000000000, -0.000000000000000000 ) ) ;
#4269 = ORIENTED_EDGE ( 'NONE', *, *, #5198, .F. ) ;
#4270 = CARTESIAN_POINT ( 'NONE',  ( 2.875000000000000888, 0.000000000000000000, -2.612499998777286780 ) ) ;
#4271 = CARTESIAN_POINT ( 'NONE',  ( -0.6866307324975363668, 3.648256581353261030, 8.313183197705237504 ) ) ;
#4272 = ORIENTED_EDGE ( 'NONE', *, *, #2086, .T. ) ;
#4273 = APPROVAL ( #6645, 'UNSPECIFIED' ) ;
#4274 = VECTOR ( 'NONE', #409, 39.37007874015748143 ) ;
#4275 = CARTESIAN_POINT ( 'NONE',  ( 0.000000000000000000, 2.325000000000000622, -3.080208333333334103 ) ) ;
#4276 = CARTESIAN_POINT ( 'NONE',  ( -1.388463899750249738E-31, 3.950000000000000178, -4.043750000000001066 ) ) ;
#4277 = CARTESIAN_POINT ( 'NONE',  ( -2.750000000000000444, 7.964000000000000412, 3.956250000000000266 ) ) ;
#4278 = EDGE_CURVE ( 'NONE', #4859, #3123, #8100, .T. ) ;
#4279 = DIRECTION ( 'NONE',  ( 0.7071067811865474617, 0.000000000000000000, 0.7071067811865474617 ) ) ;
#4280 = CARTESIAN_POINT ( 'NONE',  ( 1.187499999999999778, 5.002317768095269734, 4.083473622031662309 ) ) ;
#4281 = VERTEX_POINT ( 'NONE', #4924 ) ;
#4282 = APPLICATION_PROTOCOL_DEFINITION ( 'international standard', 'config_control_design', 1994, #5651 ) ;
#4283 = CARTESIAN_POINT ( 'NONE',  ( 0.000000000000000000, 0.000000000000000000, 3.823750000000002647 ) ) ;
#4284 = DIMENSIONAL_EXPONENTS ( 1.000000000000000000, 0.000000000000000000, 0.000000000000000000, 0.000000000000000000, 0.000000000000000000, 0.000000000000000000, 0.000000000000000000 ) ;
#4285 = ADVANCED_FACE ( 'NONE', ( #3694 ), #7463, .T. ) ;
#4286 = EDGE_LOOP ( 'NONE', ( #4189, #8050 ) ) ;
#4287 = CARTESIAN_POINT ( 'NONE',  ( -1.462953685889704536, 1.365923996832131609E-16, 3.588229579064466712 ) ) ;
#4288 = CARTESIAN_POINT ( 'NONE',  ( -4.462046614173229564, 3.753500037802127043, 8.231249998505111520 ) ) ;
#4289 = ORIENTED_EDGE ( 'NONE', *, *, #921, .F. ) ;
#4290 = APPROVAL_ROLE ( '' ) ;
#4291 = LINE ( 'NONE', #3109, #4374 ) ;
#4292 = CARTESIAN_POINT ( 'NONE',  ( -0.6563132439730009482, 5.089852872402901518, -5.108749999999999680 ) ) ;
#4293 = DATE_AND_TIME ( #2417, #7139 ) ;
#4294 = APPLICATION_CONTEXT ( 'configuration controlled 3d designs of mechanical parts and assemblies' ) ;
#4295 = CARTESIAN_POINT ( 'NONE',  ( 1.625000000000000222, 5.113999999999999879, 2.750000000234376074 ) ) ;
#4296 = DIRECTION ( 'NONE',  ( -0.000000000000000000, -0.7071067811865474617, 0.7071067811865474617 ) ) ;
#4297 = LINE ( 'NONE', #6838, #5797 ) ;
#4298 = VERTEX_POINT ( 'NONE', #5578 ) ;
#4299 = CARTESIAN_POINT ( 'NONE',  ( -0.7432847975395557860, 4.051926198797242584, 8.527359553611677967 ) ) ;
#4300 = LENGTH_MEASURE_WITH_UNIT ( LENGTH_MEASURE( 0.02539999999999999897 ), #1072 );
#4301 = DIRECTION ( 'NONE',  ( 0.000000000000000000, 1.000000000000000000, -0.000000000000000000 ) ) ;
#4302 = CARTESIAN_POINT ( 'NONE',  ( 0.000000000000000000, 5.510994133858271304, 4.968462007874015818 ) ) ;
#4303 = DATE_AND_TIME ( #1648, #7633 ) ;
#4304 = VERTEX_POINT ( 'NONE', #8142 ) ;
#4305 = CARTESIAN_POINT ( 'NONE',  ( -1.674765981361497014, 0.9999999999999978906, -3.533905824818027508 ) ) ;
#4306 = ORIENTED_EDGE ( 'NONE', *, *, #7527, .T. ) ;
#4307 = LINE ( 'NONE', #2306, #5259 ) ;
#4308 = DIRECTION ( 'NONE',  ( 0.000000000000000000, 0.000000000000000000, 1.000000000000000000 ) ) ;
#4309 = DIRECTION ( 'NONE',  ( 0.000000000000000000, -0.000000000000000000, 1.000000000000000000 ) ) ;
#4310 = ORIENTED_EDGE ( 'NONE', *, *, #8176, .F. ) ;
#4311 = VERTEX_POINT ( 'NONE', #2478 ) ;
#4312 = DIRECTION ( 'NONE',  ( -1.000000000000000000, -0.000000000000000000, 0.000000000000000000 ) ) ;
#4313 = APPROVAL ( #2472, 'UNSPECIFIED' ) ;
#4314 = CARTESIAN_POINT ( 'NONE',  ( 1.504804212598425783, 5.036377244094489392, -5.293879055118110522 ) ) ;
#4315 = PRODUCT_DEFINITION_SHAPE ( 'NONE', 'NONE',  #8187 ) ;
#4316 = CARTESIAN_POINT ( 'NONE',  ( 1.187499999999999778, 4.766431364955767691, 5.657758996208667845 ) ) ;
#4317 = ORIENTED_EDGE ( 'NONE', *, *, #7670, .F. ) ;
#4318 = APPROVAL_STATUS ( 'not_yet_approved' ) ;
#4319 = DIRECTION ( 'NONE',  ( 1.000000000000000000, 0.000000000000000000, 0.000000000000000000 ) ) ;
#4320 = CC_DESIGN_SECURITY_CLASSIFICATION ( #1579, ( #8190 ) ) ;
#4321 = ADVANCED_FACE ( 'NONE', ( #1848 ), #2511, .F. ) ;
#4322 = CARTESIAN_POINT ( 'NONE',  ( 0.4139007112234822094, 5.536672282146937185, 4.083473622047246288 ) ) ;
#4323 = EDGE_CURVE ( 'NONE', #7215, #2207, #1112, .T. ) ;
#4324 = CARTESIAN_POINT ( 'NONE',  ( 1.462953684461641091, 1.365923996832131609E-16, 3.588229578933126440 ) ) ;
#4325 = ORIENTED_EDGE ( 'NONE', *, *, #882, .F. ) ;
#4326 = DATE_AND_TIME ( #1953, #3699 ) ;
#4327 = CARTESIAN_POINT ( 'NONE',  ( 2.750000000000000888, 7.974000000000001087, 3.333750000000001990 ) ) ;
#4328 = CALENDAR_DATE ( 2026, 8, 10 ) ;
#4329 = EDGE_CURVE ( 'NONE', #3907, #41, #5646, .T. ) ;
#4330 = PLANE ( 'NONE',  #5003 ) ;
#4331 =( BOUNDED_CURVE ( )  B_SPLINE_CURVE ( 2, ( #5341, #3473, #979, #4957, #2625, #2003, #6343, #4986, #5727 ),
 .UNSPECIFIED., .F., .F. ) 
 B_SPLINE_CURVE_WITH_KNOTS ( ( 3, 2, 2, 2, 3 ),
 ( 1.235375695993373051E-14, 0.004098851372437040987, 0.03173539256035051714, 0.05937193374826417458, 0.07317982560813471316 ),
 .UNSPECIFIED. ) 
 CURVE ( )  GEOMETRIC_REPRESENTATION_ITEM ( )  RATIONAL_B_SPLINE_CURVE ( ( 0.9260057553135151442, 0.9565602018087399072, 1.000000000000000000, 0.7071067811865479058, 1.000000000000000000, 0.7071067811865479058, 1.000000000000000000, 0.8536633850130518342, 0.8535534732088589926 ) ) 
 REPRESENTATION_ITEM ( '' )  );
#4332 = ORIENTED_EDGE ( 'NONE', *, *, #6093, .T. ) ;
#4333 = CARTESIAN_POINT ( 'NONE',  ( -0.6994518761186668820, 4.220944655642501431, 8.388267944106205576 ) ) ;
#4334 = DIRECTION ( 'NONE',  ( 1.000000000000000000, 0.000000000000000000, 0.000000000000000000 ) ) ;
#4335 = CARTESIAN_POINT ( 'NONE',  ( -3.562500000000000444, -3.820994442221351629E-18, 2.975000000000000977 ) ) ;
#4336 = DIRECTION ( 'NONE',  ( -0.000000000000000000, -1.000000000000000000, 0.000000000000000000 ) ) ;
#4337 = PERSON_AND_ORGANIZATION ( #7862, #8117 ) ;
#4338 = ORIENTED_EDGE ( 'NONE', *, *, #6890, .T. ) ;
#4339 = CARTESIAN_POINT ( 'NONE',  ( -2.126102704745536975, 0.9999999999999980016, -3.279369616341864635 ) ) ;
#4340 = ORIENTED_EDGE ( 'NONE', *, *, #3118, .F. ) ;
#4341 = CARTESIAN_POINT ( 'NONE',  ( 0.000000000000000000, 5.151388682096968097, 2.749999999536767437 ) ) ;
#4342 = DIRECTION ( 'NONE',  ( 0.000000000000000000, -1.000000000000000000, 0.000000000000000000 ) ) ;
#4343 = DIRECTION ( 'NONE',  ( 1.000000000000000000, 0.000000000000000000, 0.000000000000000000 ) ) ;
#4344 = VERTEX_POINT ( 'NONE', #3807 ) ;
#4345 = ORIENTED_EDGE ( 'NONE', *, *, #6340, .F. ) ;
#4346 = EDGE_CURVE ( 'NONE', #1721, #7577, #4505, .T. ) ;
#4347 = PRODUCT_DEFINITION_FORMATION_WITH_SPECIFIED_SOURCE ( 'ANY', '', #8109, .NOT_KNOWN. ) ;
#4348 = CARTESIAN_POINT ( 'NONE',  ( 3.987953385826773278, 4.139745409976817392, 8.179444766280242973 ) ) ;
#4349 = CARTESIAN_POINT ( 'NONE',  ( -3.987046614173228587, 3.753500037802127043, 8.243275897753244763 ) ) ;
#4350 = CARTESIAN_POINT ( 'NONE',  ( -3.562500000000000444, 0.000000000000000000, 2.975000000000000977 ) ) ;
#4351 = ORIENTED_EDGE ( 'NONE', *, *, #7634, .F. ) ;
#4352 = CALENDAR_DATE ( 2026, 8, 10 ) ;
#4353 = DIRECTION ( 'NONE',  ( 0.000000000000000000, 0.000000000000000000, -1.000000000000000000 ) ) ;
#4354 = VECTOR ( 'NONE', #4268, 39.37007874015748143 ) ;
#4355 = VERTEX_POINT ( 'NONE', #5121 ) ;
#4356 = VECTOR ( 'NONE', #4203, 39.37007874015748143 ) ;
#4357 = LOCAL_TIME ( 0, 37, 23.00000000000000000, #1090 ) ;
#4358 = APPROVAL ( #7701, 'UNSPECIFIED' ) ;
#4359 = CARTESIAN_POINT ( 'NONE',  ( -0.1312789392238629671, 2.329012898157790001, -3.076250280708381801 ) ) ;
#4360 = B_SPLINE_CURVE_WITH_KNOTS ( 'NONE', 3,
 ( #6183, #4167, #5440, #8132, #2470, #4952, #7358, #5519, #567, #453, #4835, #1111, #2950, #6688, #7322, #2986, #3068, #8006, #1724, #7494, #4205, #1224, #2505, #1841, #8046, #3724, #6228, #1687, #3022, #5569, #4333, #6840, #6066, #3611, #3653, #1764, #616, #1071, #8087, #4299, #2425, #3687, #3562, #529 ),
 .UNSPECIFIED., .F., .F.,
 ( 4, 2, 2, 2, 2, 2, 2, 2, 2, 2, 2, 2, 2, 2, 2, 2, 2, 2, 2, 2, 2, 4 ),
 ( 0.02509446659736457724, 0.02666229889018166543, 0.02744621503659023035, 0.02823013118299879526, 0.02979796347581595978, 0.03058187962222452122, 0.03136579576863308960, 0.03293362806145024718, 0.03450146035426740476, 0.03528537650067598008, 0.03606929264708456234, 0.03763712493990171298, 0.03842104108631023973, 0.03920495723271877342, 0.04077278952553576447, 0.04234062181835274857, 0.04390845411116973268, 0.04547628640398672373, 0.04626020255039523660, 0.04704411869680374947, 0.04861195098962078215, 0.05017978328243780789 ),
 .UNSPECIFIED. ) ;
#4361 = DIRECTION ( 'NONE',  ( 0.000000000000000000, 0.000000000000000000, -1.000000000000000000 ) ) ;
#4362 = AXIS2_PLACEMENT_3D ( 'NONE', #3561, #6064, #450 ) ;
#4363 = EDGE_CURVE ( 'NONE', #8092, #5981, #4897, .T. ) ;
#4364 = CARTESIAN_POINT ( 'NONE',  ( 0.000000000000000000, 5.137500000000000178, 6.956250000000000711 ) ) ;
#4365 = ORIENTED_EDGE ( 'NONE', *, *, #2675, .F. ) ;
#4366 = DATE_AND_TIME ( #2574, #2796 ) ;
#4367 = LINE ( 'NONE', #2697, #6751 ) ;
#4368 = APPROVAL_ROLE ( '' ) ;
#4369 = CARTESIAN_POINT ( 'NONE',  ( 3.063407153363070012, 2.250083286129449966, 0.5624999982029994516 ) ) ;
#4370 = LINE ( 'NONE', #6876, #5718 ) ;
#4371 = VECTOR ( 'NONE', #5944, 39.37007874015748143 ) ;
#4372 = CARTESIAN_POINT ( 'NONE',  ( -3.987046614173229475, 3.773847781577545746, 8.143725961105161559 ) ) ;
#4373 = CARTESIAN_POINT ( 'NONE',  ( -2.750000000000000444, 8.729000000000002757, 3.833750000000001545 ) ) ;
#4374 = VECTOR ( 'NONE', #6796, 39.37007874015748143 ) ;
#4375 = EDGE_CURVE ( 'NONE', #674, #1793, #5779, .T. ) ;
#4376 = CARTESIAN_POINT ( 'NONE',  ( -3.987046614173228587, 3.753500037802127043, 8.231249998505111520 ) ) ;
#4377 = VERTEX_POINT ( 'NONE', #7018 ) ;
#4378 = CARTESIAN_POINT ( 'NONE',  ( -1.625000000000000222, 2.500000000000000000, 2.521780125229002412 ) ) ;
#4379 = AXIS2_PLACEMENT_3D ( 'NONE', #400, #1676, #7345 ) ;
#4380 =( LENGTH_UNIT ( ) NAMED_UNIT ( * ) SI_UNIT ( $, .METRE. ) );
#4381 = DIRECTION ( 'NONE',  ( -0.9925485533564400997, -0.000000000000000000, 0.1218497814115311745 ) ) ;
#4382 = ADVANCED_FACE ( 'NONE', ( #3774 ), #1405, .T. ) ;
#4383 = CARTESIAN_POINT ( 'NONE',  ( 3.182000000000000828, 2.359000000000000874, 3.956250000000000266 ) ) ;
#4384 = APPROVAL_STATUS ( 'not_yet_approved' ) ;
#4385 = ORIENTED_EDGE ( 'NONE', *, *, #3644, .T. ) ;
#4386 = DIRECTION ( 'NONE',  ( 0.000000000000000000, 0.7071067811865475727, -0.7071067811865475727 ) ) ;
#4387 = EDGE_CURVE ( 'NONE', #7338, #6439, #2278, .T. ) ;
#4388 = EDGE_CURVE ( 'NONE', #2954, #5429, #5700, .T. ) ;
#4389 = VECTOR ( 'NONE', #714, 39.37007874015748143 ) ;
#4390 = ORIENTED_EDGE ( 'NONE', *, *, #2443, .F. ) ;
#4391 = ORIENTED_EDGE ( 'NONE', *, *, #1210, .T. ) ;
#4392 = VECTOR ( 'NONE', #6964, 39.37007874015748143 ) ;
#4393 = CIRCLE ( 'NONE', #869, 0.3625000012227142521 ) ;
#4394 = DIRECTION ( 'NONE',  ( 1.000000000000000000, 0.000000000000000000, 0.000000000000000000 ) ) ;
#4395 = CARTESIAN_POINT ( 'NONE',  ( 0.1707770588212104701, 2.645851873985466174, -5.108749999999999680 ) ) ;
#4396 = CARTESIAN_POINT ( 'NONE',  ( 1.187500000000000888, 4.383229855599106273, 6.623918406007527793 ) ) ;
#4397 = VERTEX_POINT ( 'NONE', #5159 ) ;
#4398 = APPROVAL_ROLE ( '' ) ;
#4399 = LINE ( 'NONE', #3784, #2314 ) ;
#4400 = CARTESIAN_POINT ( 'NONE',  ( -0.7371834602650286783, 3.810622082980043679, 8.511693372783508238 ) ) ;
#4401 = CIRCLE ( 'NONE', #7156, 1.624999999999999778 ) ;
#4402 = ORIENTED_EDGE ( 'NONE', *, *, #8011, .F. ) ;
#4403 = APPLICATION_CONTEXT ( 'configuration controlled 3d designs of mechanical parts and assemblies' ) ;
#4404 = VECTOR ( 'NONE', #5183, 39.37007874015748143 ) ;
#4405 = DIRECTION ( 'NONE',  ( -0.7071067811865667796, 0.7071067811865281438, -0.000000000000000000 ) ) ;
#4406 = CARTESIAN_POINT ( 'NONE',  ( 0.7335700378700447111, 2.500000000079424911, -2.749999999768383940 ) ) ;
#4407 = ORIENTED_EDGE ( 'NONE', *, *, #3917, .F. ) ;
#4408 = PERSON_AND_ORGANIZATION_ROLE ( 'classification_officer' ) ;
#4409 = CARTESIAN_POINT ( 'NONE',  ( 4.462953385826773811, 4.225666661560476101, 8.231249998505111520 ) ) ;
#4410 = APPROVAL_ROLE ( '' ) ;
#4411 = LINE ( 'NONE', #1339, #5585 ) ;
#4412 = DIRECTION ( 'NONE',  ( -0.000000000000000000, 1.000000000000000000, -0.000000000000000000 ) ) ;
#4413 = VECTOR ( 'NONE', #1845, 39.37007874015748854 ) ;
#4414 = CARTESIAN_POINT ( 'NONE',  ( -3.063407152776790543, 2.250083286516130432, 0.5624999999177930921 ) ) ;
#4415 = CARTESIAN_POINT ( 'NONE',  ( -1.625000000000000222, 2.500000000077463369, -2.521780125186765975 ) ) ;
#4416 = CARTESIAN_POINT ( 'NONE',  ( -4.462046614173230452, 3.674333370316265057, 8.231249998505111520 ) ) ;
#4417 = ORIENTED_EDGE ( 'NONE', *, *, #7910, .F. ) ;
#4418 = CARTESIAN_POINT ( 'NONE',  ( -4.066213280839896527, 3.516000035344541974, 8.231249998505111520 ) ) ;
#4419 = CC_DESIGN_PERSON_AND_ORGANIZATION_ASSIGNMENT ( #5919, #6996, ( #5212 ) ) ;
#4420 = CARTESIAN_POINT ( 'NONE',  ( -2.750000000000000888, 8.589000000000000412, 4.404023385826772774 ) ) ;
#4421 = DATE_AND_TIME ( #1927, #4024 ) ;
#4422 = ORIENTED_EDGE ( 'NONE', *, *, #7093, .T. ) ;
#4423 = FACE_OUTER_BOUND ( 'NONE', #7421, .T. ) ;
#4424 = CARTESIAN_POINT ( 'NONE',  ( 2.375000000000004441, 2.762499999999999289, 6.956249999999992717 ) ) ;
#4425 = DIRECTION ( 'NONE',  ( -1.000000000000000000, -0.000000000000000000, -0.000000000000000000 ) ) ;
#4426 = CARTESIAN_POINT ( 'NONE',  ( 2.750000000000000444, 7.973999999999999311, 3.833750000000001545 ) ) ;
#4427 = ADVANCED_FACE ( 'NONE', ( #3158 ), #6316, .F. ) ;
#4428 = DIRECTION ( 'NONE',  ( 0.000000000000000000, 0.000000000000000000, 1.000000000000000000 ) ) ;
#4429 = ORIENTED_EDGE ( 'NONE', *, *, #7837, .F. ) ;
#4430 = ORIENTED_EDGE ( 'NONE', *, *, #3639, .F. ) ;
#4431 = CARTESIAN_POINT ( 'NONE',  ( 3.987953385826772834, 4.025408469936202493, 8.049793446537611530 ) ) ;
#4432 = CARTESIAN_POINT ( 'NONE',  ( 1.246236519039154444, 4.370643088443840085, -5.108749999999997904 ) ) ;
#4433 = DIRECTION ( 'NONE',  ( -1.000000000000000000, -0.000000000000000000, 0.000000000000000000 ) ) ;
#4434 = ORIENTED_EDGE ( 'NONE', *, *, #8133, .F. ) ;
#4435 = CARTESIAN_POINT ( 'NONE',  ( 1.625000000000000222, 0.000000000000000000, 0.000000000000000000 ) ) ;
#4436 = DIMENSIONAL_EXPONENTS ( 1.000000000000000000, 0.000000000000000000, 0.000000000000000000, 0.000000000000000000, 0.000000000000000000, 0.000000000000000000, 0.000000000000000000 ) ;
#4437 = LINE ( 'NONE', #2644, #6524 ) ;
#4438 = EDGE_LOOP ( 'NONE', ( #5490, #6105, #1781, #2520 ) ) ;
#4439 = EDGE_CURVE ( 'NONE', #7262, #5130, #155, .T. ) ;
#4440 = LINE ( 'NONE', #6556, #7151 ) ;
#4441 = CARTESIAN_POINT ( 'NONE',  ( 2.150000000000000799, 5.025000000000000355, 3.440250000000000696 ) ) ;
#4442 = DIRECTION ( 'NONE',  ( -0.000000000000000000, -0.000000000000000000, 1.000000000000000000 ) ) ;
#4443 = B_SPLINE_CURVE_WITH_KNOTS ( 'NONE', 3,
 ( #304, #4764, #4723, #5335, #1544, #7803 ),
 .UNSPECIFIED., .F., .F.,
 ( 4, 2, 4 ),
 ( 9.813077866773594792E-18, 0.007631658735546109629, 0.01526331747109221058 ),
 .UNSPECIFIED. ) ;
#4444 = APPLICATION_CONTEXT ( 'configuration controlled 3d designs of mechanical parts and assemblies' ) ;
#4445 = VERTEX_POINT ( 'NONE', #4550 ) ;
#4446 = ORIENTED_EDGE ( 'NONE', *, *, #2920, .T. ) ;
#4447 = DATE_AND_TIME ( #6, #8077 ) ;
#4448 = CARTESIAN_POINT ( 'NONE',  ( 4.470366332363715500, 1.000000000000000666, 2.937534001674282358 ) ) ;
#4449 = CALENDAR_DATE ( 2026, 8, 10 ) ;
#4450 = DIRECTION ( 'NONE',  ( -0.000000000000000000, -1.000000000000000000, -0.000000000000000000 ) ) ;
#4451 = CARTESIAN_POINT ( 'NONE',  ( -1.557862129473126966, 2.150738729911186198, 2.750000000000000444 ) ) ;
#4452 = LOCAL_TIME ( 0, 37, 23.00000000000000000, #2852 ) ;
#4453 = DIRECTION ( 'NONE',  ( -0.000000000000000000, -1.000000000000000000, -0.000000000000000000 ) ) ;
#4454 = CARTESIAN_POINT ( 'NONE',  ( 0.000000000000000000, 5.137500000000000178, 6.956250000000000711 ) ) ;
#4455 = VERTEX_POINT ( 'NONE', #1932 ) ;
#4456 = LINE ( 'NONE', #6352, #5277 ) ;
#4457 =( CONVERSION_BASED_UNIT ( 'INCH', #1925 ) LENGTH_UNIT ( ) NAMED_UNIT ( #3806 ) );
#4458 = CARTESIAN_POINT ( 'NONE',  ( 0.000000000000000000, 3.950000000000000178, 8.831250000000000711 ) ) ;
#4459 = PERSON_AND_ORGANIZATION_ROLE ( 'design_supplier' ) ;
#4460 = VERTEX_POINT ( 'NONE', #3922 ) ;
#4461 = DIRECTION ( 'NONE',  ( 0.000000000000000000, 0.000000000000000000, -1.000000000000000000 ) ) ;
#4462 = CC_DESIGN_PERSON_AND_ORGANIZATION_ASSIGNMENT ( #2385, #1768, ( #4489 ) ) ;
#4463 = CARTESIAN_POINT ( 'NONE',  ( -2.537500000000000533, 2.500000000000000444, -0.000000000000000000 ) ) ;
#4464 = CARTESIAN_POINT ( 'NONE',  ( 0.000000000000000000, 3.950000000000000178, 7.231250000000000178 ) ) ;
#4465 = LINE ( 'NONE', #7020, #4751 ) ;
#4466 = ORIENTED_EDGE ( 'NONE', *, *, #4851, .F. ) ;
#4467 = ORIENTED_EDGE ( 'NONE', *, *, #1077, .F. ) ;
#4468 = MANIFOLD_SOLID_BREP ( 'Imported1', #4774 ) ;
#4469 = CARTESIAN_POINT ( 'NONE',  ( 3.987953385826771946, 4.060302611091127112, 8.068595639695296029 ) ) ;
#4470 = CARTESIAN_POINT ( 'NONE',  ( 0.5830436418431348411, 5.126677097923686865, -5.108750000000001457 ) ) ;
#4471 = EDGE_CURVE ( 'NONE', #1186, #1434, #3098, .T. ) ;
#4472 = CARTESIAN_POINT ( 'NONE',  ( 2.537500000000000533, 2.500000000000000444, 0.4312500000000004663 ) ) ;
#4473 = DIRECTION ( 'NONE',  ( 0.000000000000000000, -1.000000000000000000, 0.000000000000000000 ) ) ;
#4474 = ADVANCED_FACE ( 'NONE', ( #114 ), #1631, .T. ) ;
#4475 = ORIENTED_EDGE ( 'NONE', *, *, #2724, .F. ) ;
#4476 = EDGE_CURVE ( 'NONE', #277, #5733, #710, .T. ) ;
#4477 = LINE ( 'NONE', #6462, #3339 ) ;
#4478 = LINE ( 'NONE', #6296, #7000 ) ;
#4479 = ORIENTED_EDGE ( 'NONE', *, *, #381, .F. ) ;
#4480 = PERSON_AND_ORGANIZATION ( #7862, #8117 ) ;
#4481 = AXIS2_PLACEMENT_3D ( 'NONE', #6423, #1510, #766 ) ;
#4482 = DIRECTION ( 'NONE',  ( 0.000000000000000000, -0.000000000000000000, 1.000000000000000000 ) ) ;
#4483 = SECURITY_CLASSIFICATION ( '', '', #672 ) ;
#4484 = APPROVAL_DATE_TIME ( #4945, #3415 ) ;
#4485 = DIRECTION ( 'NONE',  ( 1.000000000000000000, 0.000000000000000000, -0.000000000000000000 ) ) ;
#4486 = DIRECTION ( 'NONE',  ( 1.000000000000000000, 0.000000000000000000, 0.000000000000000000 ) ) ;
#4487 = CARTESIAN_POINT ( 'NONE',  ( 0.6818077110526898910, 3.637528807515572726, 8.210173163913728089 ) ) ;
#4488 = AXIS2_PLACEMENT_3D ( 'NONE', #3150, #5641, #3722 ) ;
#4489 = PRODUCT ( 'bench vise3-', 'bench vise3-', '', ( #2429 ) ) ;
#4490 = AXIS2_PLACEMENT_3D ( 'NONE', #4138, #3534, #6661 ) ;
#4491 = VERTEX_POINT ( 'NONE', #818 ) ;
#4492 = DIRECTION ( 'NONE',  ( 1.000000000000000000, 0.000000000000000000, 0.000000000000000000 ) ) ;
#4493 = DIRECTION ( 'NONE',  ( 1.000000000000000000, 0.000000000000000000, -0.000000000000000000 ) ) ;
#4494 = CARTESIAN_POINT ( 'NONE',  ( -3.987046614173228587, 3.887887077483224818, 8.417726902280634249 ) ) ;
#4495 = VERTEX_POINT ( 'NONE', #5199 ) ;
#4496 = CARTESIAN_POINT ( 'NONE',  ( 0.000000000000000000, 3.950000000000000178, 7.131250000000001421 ) ) ;
#4497 = EDGE_CURVE ( 'NONE', #445, #6962, #7745, .T. ) ;
#4498 = DIRECTION ( 'NONE',  ( 0.000000000000000000, 0.000000000000000000, 1.000000000000000000 ) ) ;
#4499 = CARTESIAN_POINT ( 'NONE',  ( -1.187499999999998002, 4.988117721439054186, 4.328788360466695018 ) ) ;
#4500 = APPROVAL_STATUS ( 'not_yet_approved' ) ;
#4501 =( BOUNDED_SURFACE ( )  B_SPLINE_SURFACE ( 3, 3, ( 
 ( #6479, #2243, #6569, #3947 ),
 ( #1023, #320, #5895, #7735 ),
 ( #6015, #2210, #7214, #5191 ),
 ( #5862, #2707, #937, #2169 ) ),
 .UNSPECIFIED., .F., .F., .T. ) 
 B_SPLINE_SURFACE_WITH_KNOTS ( ( 4, 4 ),
 ( 4, 4 ),
 ( 0.000000000000000000, 1.000000000000000000 ),
 ( 0.000000000000000000, 1.000000000000000000 ),
 .UNSPECIFIED. ) 
 GEOMETRIC_REPRESENTATION_ITEM ( )  RATIONAL_B_SPLINE_SURFACE ( (
 ( 1.000000000000000000, 0.3333333333333330373, 0.3333333333333330373, 1.000000000000000000),
 ( 0.8047378541243660477, 0.2682459513747890156, 0.2682459513747890156, 0.8047378541243660477),
 ( 0.8047378541243660477, 0.2682459513747890156, 0.2682459513747890156, 0.8047378541243660477),
 ( 1.000000000000000000, 0.3333333333333330373, 0.3333333333333330373, 1.000000000000000000) ) ) 
 REPRESENTATION_ITEM ( '' )  SURFACE ( )  );
#4502 = VERTEX_POINT ( 'NONE', #745 ) ;
#4503 = AXIS2_PLACEMENT_3D ( 'NONE', #1528, #5276, #4011 ) ;
#4504 = CARTESIAN_POINT ( 'NONE',  ( -1.201750196850394081, 2.500000000000000444, 2.750000000000000444 ) ) ;
#4505 = LINE ( 'NONE', #3883, #454 ) ;
#4506 = DIRECTION ( 'NONE',  ( -0.000000000000000000, 1.000000000000000000, -0.000000000000000000 ) ) ;
#4507 = ORIENTED_EDGE ( 'NONE', *, *, #8079, .T. ) ;
#4508 = APPROVAL ( #7810, 'UNKNOWN' ) ;
#4509 = ORIENTED_EDGE ( 'NONE', *, *, #3096, .T. ) ;
#4510 = AXIS2_PLACEMENT_3D ( 'NONE', #7130, #1519, #3312 ) ;
#4511 = ORGANIZATION ( 'NAUO-ORG4', 'UNSPECIFIED', 'UNSPECIFIED' ) ;
#4512 = CARTESIAN_POINT ( 'NONE',  ( 3.987953385826771058, 4.023873226579484097, 8.049163100252867409 ) ) ;
#4513 = CONICAL_SURFACE ( 'NONE', #205, 3.343750000040417447, 0.4297622790966887374 ) ;
#4514 = CARTESIAN_POINT ( 'NONE',  ( 1.146819099299166034, 3.311311129500751793, -5.108750000000002345 ) ) ;
#4515 = CARTESIAN_POINT ( 'NONE',  ( 0.6237442712837091285, 2.448197894244100947, -2.959338728480837233 ) ) ;
#4516 = CARTESIAN_POINT ( 'NONE',  ( 2.740000000000000213, 8.724000000000001975, 3.328750000000001652 ) ) ;
#4517 = VERTEX_POINT ( 'NONE', #3239 ) ;
#4518 = APPROVAL ( #185, 'UNSPECIFIED' ) ;
#4519 = CARTESIAN_POINT ( 'NONE',  ( 3.987953385826772834, 3.831386823445262380, 8.387951386028717593 ) ) ;
#4520 = CARTESIAN_POINT ( 'NONE',  ( 1.489119986973711507, 2.223645902782970030, 2.749999999536767437 ) ) ;
#4521 = ORIENTED_EDGE ( 'NONE', *, *, #3977, .F. ) ;
#4522 = AXIS2_PLACEMENT_3D ( 'NONE', #7892, #922, #5373 ) ;
#4523 = CARTESIAN_POINT ( 'NONE',  ( -3.343750000000002220, 2.500000000000000444, -0.5624999994010003723 ) ) ;
#4524 = LINE ( 'NONE', #1906, #2691 ) ;
#4525 = CARTESIAN_POINT ( 'NONE',  ( 0.000000000000000000, 2.661265787401576155, 3.956250000000001155 ) ) ;
#4526 = VECTOR ( 'NONE', #2328, 39.37007874015748143 ) ;
#4527 = ORIENTED_EDGE ( 'NONE', *, *, #1550, .T. ) ;
#4528 = AXIS2_PLACEMENT_3D ( 'NONE', #4825, #7346, #8032 ) ;
#4529 = DATE_AND_TIME ( #4569, #2533 ) ;
#4530 = ADVANCED_FACE ( 'NONE', ( #2631 ), #7656, .F. ) ;
#4531 = DIRECTION ( 'NONE',  ( 0.7071067811865474617, 0.000000000000000000, -0.7071067811865474617 ) ) ;
#4532 = DATE_AND_TIME ( #311, #4709 ) ;
#4533 = CARTESIAN_POINT ( 'NONE',  ( -2.740000000000001545, 7.964000000000000412, 4.313750000000002416 ) ) ;
#4534 = CARTESIAN_POINT ( 'NONE',  ( 2.815000007187132613, 1.365923996832131609E-16, -3.895000001893597741 ) ) ;
#4535 = CIRCLE ( 'NONE', #5844, 3.874999999025058539 ) ;
#4536 = VECTOR ( 'NONE', #2341, 39.37007874015748143 ) ;
#4537 = ORIENTED_EDGE ( 'NONE', *, *, #6497, .F. ) ;
#4538 = FACE_OUTER_BOUND ( 'NONE', #6320, .T. ) ;
#4539 = DIRECTION ( 'NONE',  ( 0.000000000000000000, 0.000000000000000000, 1.000000000000000000 ) ) ;
#4540 = CARTESIAN_POINT ( 'NONE',  ( -3.987046614173228587, 3.878440408003787532, 8.414258516751308647 ) ) ;
#4541 = ORIENTED_EDGE ( 'NONE', *, *, #166, .T. ) ;
#4542 = CARTESIAN_POINT ( 'NONE',  ( -2.815000008655330621, 1.365923996832131609E-16, -3.895000002097408487 ) ) ;
#4543 = ORIENTED_EDGE ( 'NONE', *, *, #4090, .T. ) ;
#4544 = CARTESIAN_POINT ( 'NONE',  ( 1.407335172284329916, 2.812660052342383477, 9.174522246685079097 ) ) ;
#4545 = CARTESIAN_POINT ( 'NONE',  ( 2.750000000000000444, 8.589000000000000412, 5.236250000000000071 ) ) ;
#4546 = FACE_OUTER_BOUND ( 'NONE', #7188, .T. ) ;
#4547 = DATE_TIME_ROLE ( 'classification_date' ) ;
#4548 = ORIENTED_EDGE ( 'NONE', *, *, #3082, .F. ) ;
#4549 = EDGE_CURVE ( 'NONE', #3004, #3267, #2252, .T. ) ;
#4550 = CARTESIAN_POINT ( 'NONE',  ( 2.740000000000000657, 8.719000000000001194, 3.823750000000002647 ) ) ;
#4551 = DIRECTION ( 'NONE',  ( 0.000000000000000000, 0.000000000000000000, 1.000000000000000000 ) ) ;
#4552 = B_SPLINE_CURVE_WITH_KNOTS ( 'NONE', 3,
 ( #8162, #1865, #4980, #553 ),
 .UNSPECIFIED., .F., .F.,
 ( 4, 4 ),
 ( 1.026013551136062230E-11, 0.01222568458709676585 ),
 .UNSPECIFIED. ) ;
#4553 = COORDINATED_UNIVERSAL_TIME_OFFSET ( 0, 0, .AHEAD. ) ;
#4554 = ORIENTED_EDGE ( 'NONE', *, *, #7921, .F. ) ;
#4555 = CARTESIAN_POINT ( 'NONE',  ( -0.6863513793485908066, 3.647607376475762386, 8.149781182892043674 ) ) ;
#4556 = EDGE_LOOP ( 'NONE', ( #7734, #512, #2963, #4390 ) ) ;
#4557 = CARTESIAN_POINT ( 'NONE',  ( 3.987953385826772834, 3.871501457987948314, 8.050987717002785260 ) ) ;
#4558 = CARTESIAN_POINT ( 'NONE',  ( 0.6563132712551269510, 2.810147165011805725, -5.108750000000004121 ) ) ;
#4559 = CARTESIAN_POINT ( 'NONE',  ( 2.946793808523474834, 2.500000000017352786, -0.5625000000000002220 ) ) ;
#4560 = APPROVAL_PERSON_ORGANIZATION ( #940, #7709, #3438 ) ;
#4561 = CARTESIAN_POINT ( 'NONE',  ( 3.987953385826772390, 4.130163526685932673, 8.309711754443199538 ) ) ;
#4562 = CARTESIAN_POINT ( 'NONE',  ( -0.6994737761126068598, 3.679106805816449999, 8.388378218819653398 ) ) ;
#4563 = ORIENTED_EDGE ( 'NONE', *, *, #3088, .F. ) ;
#4564 = PRODUCT ( 'bench vise6_2-', 'bench vise6_2-', '', ( #6558 ) ) ;
#4565 = APPROVAL ( #5645, 'UNSPECIFIED' ) ;
#4566 = CARTESIAN_POINT ( 'NONE',  ( 0.000000000000000000, 3.950000000000000178, -5.108750000000001457 ) ) ;
#4567 = CARTESIAN_POINT ( 'NONE',  ( -8.751021560936518753E-10, 1.365923996832131609E-16, 5.750408897959578548E-10 ) ) ;
#4568 = EDGE_LOOP ( 'NONE', ( #706, #1142, #3336 ) ) ;
#4569 = CALENDAR_DATE ( 2026, 8, 10 ) ;
#4570 = LINE ( 'NONE', #351, #4773 ) ;
#4571 = CONTEXT_DEPENDENT_SHAPE_REPRESENTATION ( #1792, #1359 ) ;
#4572 = CARTESIAN_POINT ( 'NONE',  ( 0.6892550738286251644, 3.654300326837817359, 8.129643686836868000 ) ) ;
#4573 = CARTESIAN_POINT ( 'NONE',  ( 0.7210672075785411472, 4.156465442921959408, 8.466050100654991084 ) ) ;
#4574 = CARTESIAN_POINT ( 'NONE',  ( 0.7499999999999993339, 3.950000000000000178, 7.918749999999998401 ) ) ;
#4575 = ADVANCED_FACE ( 'NONE', ( #2299 ), #4793, .T. ) ;
#4576 = ORIENTED_EDGE ( 'NONE', *, *, #2407, .T. ) ;
#4577 = CARTESIAN_POINT ( 'NONE',  ( -3.987046614173227699, 4.025408469936037292, 8.412706550472611511 ) ) ;
#4578 = ORIENTED_EDGE ( 'NONE', *, *, #730, .F. ) ;
#4579 = CARTESIAN_POINT ( 'NONE',  ( -1.500000000000000444, 3.950000000000000178, 2.749999998413802160 ) ) ;
#4580 = EDGE_LOOP ( 'NONE', ( #2642, #8020 ) ) ;
#4581 = DIRECTION ( 'NONE',  ( 0.000000000000000000, 0.000000000000000000, 1.000000000000000000 ) ) ;
#4582 = DIRECTION ( 'NONE',  ( -0.000000000000000000, -0.000000000000000000, -1.000000000000000000 ) ) ;
#4583 = EDGE_CURVE ( 'NONE', #3034, #1857, #2180, .T. ) ;
#4584 = DIRECTION ( 'NONE',  ( -0.000000000000000000, -0.000000000000000000, 1.000000000000000000 ) ) ;
#4585 = COORDINATED_UNIVERSAL_TIME_OFFSET ( 0, 0, .AHEAD. ) ;
#4586 = ORIENTED_EDGE ( 'NONE', *, *, #2367, .F. ) ;
#4587 = LOCAL_TIME ( 0, 37, 23.00000000000000000, #137 ) ;
#4588 = EDGE_CURVE ( 'NONE', #605, #5981, #1480, .T. ) ;
#4589 = EDGE_CURVE ( 'NONE', #2473, #5196, #3444, .T. ) ;
#4590 = CARTESIAN_POINT ( 'NONE',  ( -1.146819095829421098, 4.588688891394698821, -5.108749999999999680 ) ) ;
#4591 = DIRECTION ( 'NONE',  ( 0.000000000000000000, 0.000000000000000000, -1.000000000000000000 ) ) ;
#4592 =( LENGTH_UNIT ( ) NAMED_UNIT ( * ) SI_UNIT ( $, .METRE. ) );
#4593 = LINE ( 'NONE', #3966, #7133 ) ;
#4594 = ORIENTED_EDGE ( 'NONE', *, *, #5224, .T. ) ;
#4595 = APPROVAL_STATUS ( 'not_yet_approved' ) ;
#4596 = VERTEX_POINT ( 'NONE', #253 ) ;
#4597 = MANIFOLD_SOLID_BREP ( 'Imported1', #2817 ) ;
#4598 = CARTESIAN_POINT ( 'NONE',  ( 3.987953385826772834, 3.882766440201302682, 8.046596944803717122 ) ) ;
#4599 = CARTESIAN_POINT ( 'NONE',  ( 1.462953684461640202, 1.365923996832131609E-16, 3.588229578933126884 ) ) ;
#4600 = ORIENTED_EDGE ( 'NONE', *, *, #5480, .T. ) ;
#4601 = LINE ( 'NONE', #1499, #3176 ) ;
#4602 = EDGE_LOOP ( 'NONE', ( #3772, #4594, #2751, #8069 ) ) ;
#4603 = APPLICATION_CONTEXT ( 'configuration controlled 3d designs of mechanical parts and assemblies' ) ;
#4604 = DIRECTION ( 'NONE',  ( 1.000000000000000000, 0.000000000000000000, -0.000000000000000000 ) ) ;
#4605 = ORIENTED_EDGE ( 'NONE', *, *, #1980, .T. ) ;
#4606 = DATE_AND_TIME ( #5180, #6846 ) ;
#4607 = DIRECTION ( 'NONE',  ( -0.000000000000000000, -0.000000000000000000, 1.000000000000000000 ) ) ;
#4608 = DATE_TIME_ROLE ( 'classification_date' ) ;
#4609 = FACE_BOUND ( 'NONE', #4580, .T. ) ;
#4610 = CARTESIAN_POINT ( 'NONE',  ( 0.7188803599037373315, 4.163931010176847636, 8.459265585397703902 ) ) ;
#4611 = LINE ( 'NONE', #6522, #2964 ) ;
#4612 = ORIENTED_EDGE ( 'NONE', *, *, #5840, .F. ) ;
#4613 = CARTESIAN_POINT ( 'NONE',  ( -3.987046614173228587, 4.116323182045732665, 8.335940882964735010 ) ) ;
#4614 = ORIENTED_EDGE ( 'NONE', *, *, #5686, .T. ) ;
#4615 = LINE ( 'NONE', #4734, #3844 ) ;
#4616 = MANIFOLD_SOLID_BREP ( 'N', #6353 ) ;
#4617 =( NAMED_UNIT ( * ) PLANE_ANGLE_UNIT ( ) SI_UNIT ( $, .RADIAN. ) );
#4618 = DIRECTION ( 'NONE',  ( 0.000000000000000000, 0.000000000000000000, 1.000000000000000000 ) ) ;
#4619 = CARTESIAN_POINT ( 'NONE',  ( -0.7335700378053525705, 2.500000000126119559, -5.108750000000001457 ) ) ;
#4620 = CALENDAR_DATE ( 2026, 8, 10 ) ;
#4621 = ORIENTED_EDGE ( 'NONE', *, *, #4183, .T. ) ;
#4622 = CIRCLE ( 'NONE', #3955, 2.845000000000001528 ) ;
#4623 = CC_DESIGN_APPROVAL ( #6489, ( #1030 ) ) ;
#4624 = DIRECTION ( 'NONE',  ( 0.000000000000000000, 1.000000000000000000, 0.000000000000000000 ) ) ;
#4625 = EDGE_CURVE ( 'NONE', #5748, #6859, #5992, .T. ) ;
#4626 = CIRCLE ( 'NONE', #8096, 1.624999995942718156 ) ;
#4627 = PLANE ( 'NONE',  #4503 ) ;
#4628 = AXIS2_PLACEMENT_3D ( 'NONE', #290, #4128, #2748 ) ;
#4629 =( LENGTH_UNIT ( ) NAMED_UNIT ( * ) SI_UNIT ( $, .METRE. ) );
#4630 = CYLINDRICAL_SURFACE ( 'NONE', #2929, 0.3625000012227142521 ) ;
#4631 = EDGE_LOOP ( 'NONE', ( #4935, #2255, #798, #4016 ) ) ;
#4632 = COORDINATED_UNIVERSAL_TIME_OFFSET ( 0, 0, .AHEAD. ) ;
#4633 = ORIENTED_EDGE ( 'NONE', *, *, #1479, .T. ) ;
#4634 = EDGE_CURVE ( 'NONE', #5899, #2392, #2871, .T. ) ;
#4635 = CARTESIAN_POINT ( 'NONE',  ( -0.7333924044284376720, 3.792775136080777543, 7.960989307084957112 ) ) ;
#4636 = DIRECTION ( 'NONE',  ( 0.7071067811865475727, 0.000000000000000000, 0.7071067811865475727 ) ) ;
#4637 = AXIS2_PLACEMENT_3D ( 'NONE', #2740, #7904, #4697 ) ;
#4638 = FACE_OUTER_BOUND ( 'NONE', #5758, .T. ) ;
#4639 = CARTESIAN_POINT ( 'NONE',  ( 4.383786719160105427, 4.383999996532200072, 7.363250037317454755 ) ) ;
#4640 = CARTESIAN_POINT ( 'NONE',  ( 3.987953385826773278, 3.925026340410263881, 8.427747322941383956 ) ) ;
#4641 = EDGE_CURVE ( 'NONE', #4731, #4304, #5358, .T. ) ;
#4642 = APPROVAL_PERSON_ORGANIZATION ( #7604, #1614, #1956 ) ;
#4643 = ORIENTED_EDGE ( 'NONE', *, *, #6970, .F. ) ;
#4644 = VECTOR ( 'NONE', #3299, 39.37007874015748143 ) ;
#4645 = APPROVAL_PERSON_ORGANIZATION ( #1592, #4508, #846 ) ;
#4646 = DIRECTION ( 'NONE',  ( 0.000000000000000000, -0.000000000000000000, -1.000000000000000000 ) ) ;
#4647 = DIRECTION ( 'NONE',  ( 0.000000000000000000, 0.000000000000000000, 1.000000000000000000 ) ) ;
#4648 = APPROVAL_ROLE ( '' ) ;
#4649 = DIRECTION ( 'NONE',  ( -1.000000000000000000, 0.000000000000000000, -0.000000000000000000 ) ) ;
#4650 = SECURITY_CLASSIFICATION_LEVEL ( 'unclassified' ) ;
#4651 = CARTESIAN_POINT ( 'NONE',  ( -8.751021560936518753E-10, 1.000000000000000222, 5.750408897959578548E-10 ) ) ;
#4652 = B_SPLINE_CURVE_WITH_KNOTS ( 'NONE', 3,
 ( #6125, #3037, #3700, #1822 ),
 .UNSPECIFIED., .F., .F.,
 ( 4, 4 ),
 ( 4.860009891584967381E-13, 0.02101476597452160006 ),
 .UNSPECIFIED. ) ;
#4653 = ORIENTED_EDGE ( 'NONE', *, *, #3431, .F. ) ;
#4654 = FACE_OUTER_BOUND ( 'NONE', #5543, .T. ) ;
#4655 = CARTESIAN_POINT ( 'NONE',  ( -3.987046614173229919, 3.862475978533526089, 8.407402232862935421 ) ) ;
#4656 = ORIENTED_EDGE ( 'NONE', *, *, #4691, .T. ) ;
#4657 = CARTESIAN_POINT ( 'NONE',  ( 3.562500000000000444, -3.820994442221351629E-18, 2.975000000000000977 ) ) ;
#4658 = EDGE_LOOP ( 'NONE', ( #816, #7742, #6644, #6140 ) ) ;
#4659 = DIRECTION ( 'NONE',  ( 0.0005594472316432187384, -8.183956524382560936E-17, 0.9999998435093852001 ) ) ;
#4660 = DIRECTION ( 'NONE',  ( 0.000000000000000000, -0.000000000000000000, 1.000000000000000000 ) ) ;
#4661 = EDGE_CURVE ( 'NONE', #1998, #2981, #2016, .T. ) ;
#4662 = PERSON_AND_ORGANIZATION ( #7862, #8117 ) ;
#4663 = ORIENTED_EDGE ( 'NONE', *, *, #2598, .T. ) ;
#4664 = AXIS2_PLACEMENT_3D ( 'NONE', #236, #3265, #7044 ) ;
#4665 = AXIS2_PLACEMENT_3D ( 'NONE', #6972, #4342, #1284 ) ;
#4666 = DIRECTION ( 'NONE',  ( 0.000000000000000000, 0.7071067811865474617, -0.7071067811865474617 ) ) ;
#4667 = CARTESIAN_POINT ( 'NONE',  ( -1.113928750309983506, 4.644468174584341469, -5.108750000000003233 ) ) ;
#4668 = CARTESIAN_POINT ( 'NONE',  ( -0.4482830794785033768, 2.386743749610857002, 3.019476368352826956 ) ) ;
#4669 = CC_DESIGN_DATE_AND_TIME_ASSIGNMENT ( #2402, #546, ( #2668 ) ) ;
#4670 = DIRECTION ( 'NONE',  ( -0.9531066744720206874, 0.000000000000000000, 0.3026345437601031252 ) ) ;
#4671 = DIRECTION ( 'NONE',  ( 0.000000000000000000, 0.000000000000000000, -1.000000000000000000 ) ) ;
#4672 = ORIENTED_EDGE ( 'NONE', *, *, #379, .F. ) ;
#4673 = DATE_AND_TIME ( #5996, #5404 ) ;
#4674 = VERTEX_POINT ( 'NONE', #1565 ) ;
#4675 = ADVANCED_FACE ( 'NONE', ( #7915 ), #5903, .F. ) ;
#4676 = ADVANCED_FACE ( 'NONE', ( #6653 ), #5235, .T. ) ;
#4677 = FACE_OUTER_BOUND ( 'NONE', #5968, .T. ) ;
#4678 = FACE_OUTER_BOUND ( 'NONE', #1450, .T. ) ;
#4679 = CARTESIAN_POINT ( 'NONE',  ( -2.750000000000000444, 7.964000000000000412, 3.823750000000002647 ) ) ;
#4680 = CARTESIAN_POINT ( 'NONE',  ( 3.987953385826772390, 4.132117433205379164, 8.305060267424163811 ) ) ;
#4681 = VERTEX_POINT ( 'NONE', #2903 ) ;
#4682 = CARTESIAN_POINT ( 'NONE',  ( -3.987046614173229919, 4.146499994074617668, 8.219224099255814764 ) ) ;
#4683 = DIRECTION ( 'NONE',  ( -0.000000000000000000, 1.000000000000000000, -0.000000000000000000 ) ) ;
#4684 = CARTESIAN_POINT ( 'NONE',  ( -1.124999999999999556, 3.950000000000000178, 7.131250000000001421 ) ) ;
#4685 = CARTESIAN_POINT ( 'NONE',  ( -2.750000000000000444, 7.964000000000001300, 4.323750000000003091 ) ) ;
#4686 = APPROVAL_ROLE ( '' ) ;
#4687 = LINE ( 'NONE', #2238, #3207 ) ;
#4688 = LINE ( 'NONE', #273, #1905 ) ;
#4689 = ADVANCED_FACE ( 'NONE', ( #5398, #7956 ), #4627, .T. ) ;
#4690 = DATE_AND_TIME ( #6470, #5425 ) ;
#4691 = EDGE_CURVE ( 'NONE', #1965, #5413, #6580, .T. ) ;
#4692 = CARTESIAN_POINT ( 'NONE',  ( 0.6866307324975362558, 4.251743418646740658, 8.313183197705233951 ) ) ;
#4693 = FACE_OUTER_BOUND ( 'NONE', #7507, .T. ) ;
#4694 = ORIENTED_EDGE ( 'NONE', *, *, #8133, .T. ) ;
#4695 = CARTESIAN_POINT ( 'NONE',  ( -1.889618362131626726E-10, 3.950000000000000178, 2.750000000234376074 ) ) ;
#4696 = EDGE_LOOP ( 'NONE', ( #1190, #752, #1880, #6513 ) ) ;
#4697 = DIRECTION ( 'NONE',  ( 1.000000000000000000, 0.000000000000000000, 0.000000000000000000 ) ) ;
#4698 = CYLINDRICAL_SURFACE ( 'NONE', #1407, 0.2625000000000008438 ) ;
#4699 = ORIENTED_EDGE ( 'NONE', *, *, #6601, .T. ) ;
#4700 =( CONVERSION_BASED_UNIT ( 'INCH', #284 ) LENGTH_UNIT ( ) NAMED_UNIT ( #88 ) );
#4701 = PLANE ( 'NONE',  #3851 ) ;
#4702 = PERSON_AND_ORGANIZATION ( #7862, #8117 ) ;
#4703 = ADVANCED_FACE ( 'NONE', ( #7830 ), #7183, .F. ) ;
#4704 = ORIENTED_EDGE ( 'NONE', *, *, #3130, .T. ) ;
#4705 = CARTESIAN_POINT ( 'NONE',  ( -1.295380381263955716, 3.737605818698255700, -5.108749999999998792 ) ) ;
#4706 = CARTESIAN_POINT ( 'NONE',  ( 0.3222455737775520856, 2.355994570478443517, 3.049679287146744411 ) ) ;
#4707 = PLANE ( 'NONE',  #6484 ) ;
#4708 =( CONVERSION_BASED_UNIT ( 'INCH', #7878 ) LENGTH_UNIT ( ) NAMED_UNIT ( #3762 ) );
#4709 = LOCAL_TIME ( 0, 37, 23.00000000000000000, #7165 ) ;
#4710 = CARTESIAN_POINT ( 'NONE',  ( -3.875000000000001332, 1.000000000000000222, 7.750000000000002665 ) ) ;
#4711 = PERSON_AND_ORGANIZATION ( #7862, #8117 ) ;
#4712 = EDGE_LOOP ( 'NONE', ( #1096, #1763 ) ) ;
#4713 = CARTESIAN_POINT ( 'NONE',  ( -3.875000000000003109, 1.000000000000000222, -7.750000000000002665 ) ) ;
#4714 = APPROVAL ( #6248, 'UNSPECIFIED' ) ;
#4715 = UNCERTAINTY_MEASURE_WITH_UNIT (LENGTH_MEASURE( 1.000000000000000082E-05 ), #6311, 'distance_accuracy_value', 'NONE');
#4716 = DIRECTION ( 'NONE',  ( 0.000000000000000000, -1.000000000000000000, -0.000000000000000000 ) ) ;
#4717 = CARTESIAN_POINT ( 'NONE',  ( 2.750000000000000444, 7.973999999999999311, 3.833750000000001545 ) ) ;
#4718 = ORIENTED_EDGE ( 'NONE', *, *, #501, .T. ) ;
#4719 = CYLINDRICAL_SURFACE ( 'NONE', #5655, 0.1875000000000006661 ) ;
#4720 = ORIENTED_EDGE ( 'NONE', *, *, #1133, .F. ) ;
#4721 = ADVANCED_FACE ( 'NONE', ( #2829 ), #4707, .T. ) ;
#4722 = CARTESIAN_POINT ( 'NONE',  ( -3.987046614173228143, 4.019420561376825241, 8.047419037877350689 ) ) ;
#4723 = CARTESIAN_POINT ( 'NONE',  ( 1.489119987881815765, 2.223645901847905115, -2.749999999536767437 ) ) ;
#4724 = EDGE_CURVE ( 'NONE', #4460, #8086, #4360, .T. ) ;
#4725 = PLANE ( 'NONE',  #460 ) ;
#4726 = PERSON_AND_ORGANIZATION ( #7862, #8117 ) ;
#4727 = CARTESIAN_POINT ( 'NONE',  ( -1.312500000051465499, 4.908106857156239400, 2.749999995422029553 ) ) ;
#4728 = CARTESIAN_POINT ( 'NONE',  ( 0.6829499219002715948, 4.259968811991060811, 8.190215189619561187 ) ) ;
#4729 = CARTESIAN_POINT ( 'NONE',  ( 0.000000000000000000, 2.499999998868537521, 0.000000000000000000 ) ) ;
#4730 = EDGE_CURVE ( 'NONE', #1442, #6928, #4917, .T. ) ;
#4731 = VERTEX_POINT ( 'NONE', #2342 ) ;
#4732 = CARTESIAN_POINT ( 'NONE',  ( 0.000000000000000000, 2.389005866141733492, 4.968462007874015818 ) ) ;
#4733 = ORIENTED_EDGE ( 'NONE', *, *, #6291, .T. ) ;
#4734 = CARTESIAN_POINT ( 'NONE',  ( 0.000000000000000000, 1.664000000000000368, 2.841000000000000636 ) ) ;
#4735 = ORIENTED_EDGE ( 'NONE', *, *, #7938, .T. ) ;
#4736 = COORDINATED_UNIVERSAL_TIME_OFFSET ( 0, 0, .AHEAD. ) ;
#4737 = CARTESIAN_POINT ( 'NONE',  ( -3.562500000000000444, 1.000000000000000222, 2.975000000000000977 ) ) ;
#4738 = COORDINATED_UNIVERSAL_TIME_OFFSET ( 0, 0, .AHEAD. ) ;
#4739 = ORIENTED_EDGE ( 'NONE', *, *, #5093, .T. ) ;
#4740 = CARTESIAN_POINT ( 'NONE',  ( -2.513411990276539942, 1.000000000000000444, -2.949302488239234243 ) ) ;
#4741 = PRODUCT_DEFINITION_FORMATION_WITH_SPECIFIED_SOURCE ( 'ANY', '', #3255, .NOT_KNOWN. ) ;
#4742 = CARTESIAN_POINT ( 'NONE',  ( -1.310546130307260748, 3.866374246920377900, -5.108750000000002345 ) ) ;
#4743 = DIRECTION ( 'NONE',  ( 0.000000000000000000, -1.000000000000000000, -0.000000000000000000 ) ) ;
#4744 = DIRECTION ( 'NONE',  ( 0.000000000000000000, 0.000000000000000000, -1.000000000000000000 ) ) ;
#4745 = VECTOR ( 'NONE', #1615, 39.37007874015748854 ) ;
#4746 = PERSON_AND_ORGANIZATION ( #7862, #8117 ) ;
#4747 = ORIENTED_EDGE ( 'NONE', *, *, #4193, .F. ) ;
#4748 = VECTOR ( 'NONE', #3301, 39.37007874015748143 ) ;
#4749 = CARTESIAN_POINT ( 'NONE',  ( 3.583510604133040900, 1.543025754838327046, -8.777069582124253846E-16 ) ) ;
#4750 = APPROVAL_PERSON_ORGANIZATION ( #7553, #3215, #3135 ) ;
#4751 = VECTOR ( 'NONE', #255, 39.37007874015748143 ) ;
#4752 = VECTOR ( 'NONE', #5835, 39.37007874015748143 ) ;
#4753 = LOCAL_TIME ( 0, 37, 23.00000000000000000, #6494 ) ;
#4754 = DIRECTION ( 'NONE',  ( 0.000000000000000000, 0.000000000000000000, 1.000000000000000000 ) ) ;
#4755 = CC_DESIGN_DATE_AND_TIME_ASSIGNMENT ( #5020, #5102, ( #5167 ) ) ;
#4756 = DIRECTION ( 'NONE',  ( 0.000000000000000000, 0.000000000000000000, -1.000000000000000000 ) ) ;
#4757 = CARTESIAN_POINT ( 'NONE',  ( 0.000000000000000000, 5.137500000000000178, 6.956250000000000711 ) ) ;
#4758 = DIRECTION ( 'NONE',  ( 1.000000000000000000, 0.000000000000000000, 0.000000000000000000 ) ) ;
#4759 =( BOUNDED_SURFACE ( )  B_SPLINE_SURFACE ( 3, 3, ( 
 ( #2221, #2300, #4710, #4794 ),
 ( #7226, #7323, #1609, #4084 ),
 ( #6621, #7916, #4170, #6690 ),
 ( #6268, #5442, #3120, #8048 ) ),
 .UNSPECIFIED., .F., .F., .F. ) 
 B_SPLINE_SURFACE_WITH_KNOTS ( ( 4, 4 ),
 ( 4, 4 ),
 ( 0.000000000000000000, 1.000000000000000000 ),
 ( 0.000000000000000000, 1.000000000000000000 ),
 .UNSPECIFIED. ) 
 GEOMETRIC_REPRESENTATION_ITEM ( )  RATIONAL_B_SPLINE_SURFACE ( (
 ( 1.000000000000000000, 0.3333333333333334259, 0.3333333333333334259, 1.000000000000000000),
 ( 1.000000000000000000, 0.3333333333333334259, 0.3333333333333334259, 1.000000000000000000),
 ( 1.000000000000000000, 0.3333333333333334259, 0.3333333333333334259, 1.000000000000000000),
 ( 1.000000000000000000, 0.3333333333333334259, 0.3333333333333334259, 1.000000000000000000) ) ) 
 REPRESENTATION_ITEM ( '' )  SURFACE ( )  );
#4760 = ORIENTED_EDGE ( 'NONE', *, *, #4583, .F. ) ;
#4761 = VECTOR ( 'NONE', #3281, 39.37007874015748143 ) ;
#4762 = EDGE_CURVE ( 'NONE', #3927, #4281, #6803, .T. ) ;
#4763 = CARTESIAN_POINT ( 'NONE',  ( -3.987046614173228587, 4.135047251020795400, 8.164838062277185671 ) ) ;
#4764 = CARTESIAN_POINT ( 'NONE',  ( 1.557862130685455426, 2.150738729487894130, -2.749999999536767437 ) ) ;
#4765 = CC_DESIGN_PERSON_AND_ORGANIZATION_ASSIGNMENT ( #2973, #7982, ( #2798 ) ) ;
#4766 = CARTESIAN_POINT ( 'NONE',  ( 0.4466248239349933646, 2.387262647126640047, -3.018973216062835085 ) ) ;
#4767 = CARTESIAN_POINT ( 'NONE',  ( 1.312500000000000444, 4.908106850393701315, 0.5414159055118112907 ) ) ;
#4768 = LINE ( 'NONE', #7296, #7289 ) ;
#4769 = ORIENTED_EDGE ( 'NONE', *, *, #2354, .T. ) ;
#4770 = DATE_AND_TIME ( #4147, #5931 ) ;
#4771 = CARTESIAN_POINT ( 'NONE',  ( 3.362500000000000711, 1.750000000000000444, -4.117874862132976456E-16 ) ) ;
#4772 = CARTESIAN_POINT ( 'NONE',  ( 0.7370170160409599269, 4.089247961470974246, 7.951302674248321267 ) ) ;
#4773 = VECTOR ( 'NONE', #4607, 39.37007874015748143 ) ;
#4774 = CLOSED_SHELL ( 'NONE', ( #7230, #493, #1137, #2187 ) ) ;
#4775 = SECURITY_CLASSIFICATION ( '', '', #6832 ) ;
#4776 = EDGE_CURVE ( 'NONE', #3375, #2544, #7453, .T. ) ;
#4777 = ORIENTED_EDGE ( 'NONE', *, *, #8044, .F. ) ;
#4778 = CARTESIAN_POINT ( 'NONE',  ( 2.815000007187132613, 1.365923996832131609E-16, -3.895000001893597297 ) ) ;
#4779 = ADVANCED_FACE ( 'NONE', ( #5484 ), #33, .T. ) ;
#4780 = ORIENTED_EDGE ( 'NONE', *, *, #6084, .T. ) ;
#4781 = CARTESIAN_POINT ( 'NONE',  ( -4.462046614173230452, 3.674333370316265057, 8.231249998505111520 ) ) ;
#4782 = PLANE ( 'NONE',  #2056 ) ;
#4783 = VERTEX_POINT ( 'NONE', #4378 ) ;
#4784 = CALENDAR_DATE ( 2026, 8, 10 ) ;
#4785 = LINE ( 'NONE', #6481, #5955 ) ;
#4786 = APPROVAL_PERSON_ORGANIZATION ( #5511, #4273, #2414 ) ;
#4787 = CARTESIAN_POINT ( 'NONE',  ( 3.562500000000000444, -0.000000000000000000, 3.337500000000003020 ) ) ;
#4788 = EDGE_LOOP ( 'NONE', ( #2997, #2513, #204, #2658 ) ) ;
#4789 = CARTESIAN_POINT ( 'NONE',  ( -2.750000000000000444, 7.964000000000000412, 3.691250000000001030 ) ) ;
#4790 = DIRECTION ( 'NONE',  ( -0.000000000000000000, -1.000000000000000000, -0.000000000000000000 ) ) ;
#4791 = CARTESIAN_POINT ( 'NONE',  ( -0.7977802270736898960, 4.992433491425203762, -5.108750000000001457 ) ) ;
#4792 = CARTESIAN_POINT ( 'NONE',  ( -0.06688424724377287078, 2.325058188798388770, 3.080150965287773879 ) ) ;
#4793 = PLANE ( 'NONE',  #1370 ) ;
#4794 = CARTESIAN_POINT ( 'NONE',  ( -3.875000000000002220, 1.000000000000000222, 4.745506346695996852E-16 ) ) ;
#4795 = COORDINATED_UNIVERSAL_TIME_OFFSET ( 0, 0, .AHEAD. ) ;
#4796 = ORIENTED_EDGE ( 'NONE', *, *, #3020, .F. ) ;
#4797 = FACE_OUTER_BOUND ( 'NONE', #1852, .T. ) ;
#4798 = CARTESIAN_POINT ( 'NONE',  ( 2.875000000000000888, 1.000000000000000222, -2.612499998777286780 ) ) ;
#4799 = EDGE_CURVE ( 'NONE', #1965, #805, #6710, .T. ) ;
#4800 = DESIGN_CONTEXT ( 'detailed design', #7847, 'design' ) ;
#4801 = AXIS2_PLACEMENT_3D ( 'NONE', #1594, #6598, #6473 ) ;
#4802 = AXIS2_PLACEMENT_3D ( 'NONE', #1830, #6827, #3175 ) ;
#4803 = DIRECTION ( 'NONE',  ( -0.7071067811865475727, 0.000000000000000000, -0.7071067811865475727 ) ) ;
#4804 = CARTESIAN_POINT ( 'NONE',  ( 1.462953684461641091, 1.365923996832131609E-16, 3.588229578933126884 ) ) ;
#4805 = CARTESIAN_POINT ( 'NONE',  ( 2.724999998660272205, 3.550000000000001155, -0.3883559095726498156 ) ) ;
#4806 = ORIENTED_EDGE ( 'NONE', *, *, #7199, .T. ) ;
#4807 = DIRECTION ( 'NONE',  ( 1.000000000000000000, -0.000000000000000000, -0.000000000000000000 ) ) ;
#4808 = ORIENTED_EDGE ( 'NONE', *, *, #5242, .T. ) ;
#4809 = B_SPLINE_CURVE_WITH_KNOTS ( 'NONE', 3,
 ( #7914, #2251, #6026, #5397, #4668, #5319, #2179, #7267, #4166, #7875, #4792, #7182, #2947, #3443, #1607, #5439, #2219, #3490, #4706, #8005, #4082, #4833, #5991, #289, #7223, #368 ),
 .UNSPECIFIED., .F., .F.,
 ( 4, 2, 2, 2, 2, 2, 2, 2, 2, 2, 2, 2, 4 ),
 ( 0.000000000000000000, 0.004967431915087203512, 0.009934863830174412228, 0.01241857978771801312, 0.01490229574526161921, 0.01986972766034882792, 0.02111158563912063010, 0.02235344361789242881, 0.02483715957543602970, 0.02980459149052323842, 0.03228830744806682890, 0.03477202340561042632, 0.03973945532069762115 ),
 .UNSPECIFIED. ) ;
#4810 = CARTESIAN_POINT ( 'NONE',  ( -3.987046614173229919, 4.143082812052600872, 8.194756059061747422 ) ) ;
#4811 = CARTESIAN_POINT ( 'NONE',  ( -2.750000000000000888, 7.964000000000000412, 3.823750000000002647 ) ) ;
#4812 = FACE_OUTER_BOUND ( 'NONE', #490, .T. ) ;
#4813 = SHAPE_REPRESENTATION ( 'bench vise-', ( #7272 ), #3062 ) ;
#4815 = APPROVAL_STATUS ( 'not_yet_approved' ) ;
#4814 = CC_DESIGN_APPROVAL ( #4565, ( #6424 ) ) ;
#4816 = LINE ( 'NONE', #5423, #5043 ) ;
#4817 = CARTESIAN_POINT ( 'NONE',  ( -0.7052155605301347885, 5.414000000000000590, 0.1249999999999998335 ) ) ;
#4818 = CC_DESIGN_PERSON_AND_ORGANIZATION_ASSIGNMENT ( #6167, #4936, ( #5745 ) ) ;
#4819 = ORIENTED_EDGE ( 'NONE', *, *, #1930, .F. ) ;
#4820 = DIRECTION ( 'NONE',  ( -0.000000000000000000, 1.000000000000000000, -0.000000000000000000 ) ) ;
#4821 = APPLICATION_CONTEXT ( 'configuration controlled 3d designs of mechanical parts and assemblies' ) ;
#4822 = EDGE_CURVE ( 'NONE', #8018, #3927, #2048, .T. ) ;
#4823 = DIRECTION ( 'NONE',  ( 0.000000000000000000, 1.000000000000000000, 0.000000000000000000 ) ) ;
#4824 = FACE_OUTER_BOUND ( 'NONE', #3691, .T. ) ;
#4825 = CARTESIAN_POINT ( 'NONE',  ( 0.000000000000000000, 3.950000000000000178, 8.981250000000001066 ) ) ;
#4826 = ORIENTED_EDGE ( 'NONE', *, *, #7420, .T. ) ;
#4827 = COORDINATED_UNIVERSAL_TIME_OFFSET ( 0, 0, .AHEAD. ) ;
#4828 = CARTESIAN_POINT ( 'NONE',  ( 4.383786719160105427, 4.383999996532202736, 9.099249959692766510 ) ) ;
#4829 = APPROVAL_STATUS ( 'not_yet_approved' ) ;
#4830 = EDGE_LOOP ( 'NONE', ( #7372, #7104, #3616, #6157 ) ) ;
#4831 = CARTESIAN_POINT ( 'NONE',  ( -1.187500000000000444, 7.339000000000001300, 4.486250000000000959 ) ) ;
#4832 = CARTESIAN_POINT ( 'NONE',  ( 1.500000000000000444, 5.339000000000000412, -2.750000000000000444 ) ) ;
#4833 = CARTESIAN_POINT ( 'NONE',  ( 0.5066049570144357528, 2.405661888747006927, 3.000938696051032473 ) ) ;
#4834 = EDGE_CURVE ( 'NONE', #5456, #3375, #2930, .T. ) ;
#4835 = CARTESIAN_POINT ( 'NONE',  ( -0.7253671533374043134, 4.140809826333097021, 7.983559312723937929 ) ) ;
#4836 =( NAMED_UNIT ( * ) PLANE_ANGLE_UNIT ( ) SI_UNIT ( $, .RADIAN. ) );
#4837 = DIRECTION ( 'NONE',  ( -0.000000000000000000, -1.000000000000000000, -0.000000000000000000 ) ) ;
#4838 = EDGE_CURVE ( 'NONE', #2112, #7591, #6267, .T. ) ;
#4839 = APPROVAL_DATE_TIME ( #8049, #7758 ) ;
#4840 = ORIENTED_EDGE ( 'NONE', *, *, #5427, .T. ) ;
#4841 = LINE ( 'NONE', #2256, #3363 ) ;
#4842 = EDGE_CURVE ( 'NONE', #2216, #4886, #3973, .T. ) ;
#4843 = LINE ( 'NONE', #8014, #2924 ) ;
#4844 = DIRECTION ( 'NONE',  ( -0.000000000000000000, -1.000000000000000000, -0.000000000000000000 ) ) ;
#4845 = ORIENTED_EDGE ( 'NONE', *, *, #7527, .F. ) ;
#4846 = DIRECTION ( 'NONE',  ( 5.213780441972162403E-17, 0.000000000000000000, -1.000000000000000000 ) ) ;
#4847 = ORIENTED_EDGE ( 'NONE', *, *, #5828, .T. ) ;
#4848 = B_SPLINE_CURVE_WITH_KNOTS ( 'NONE', 3,
 ( #4987, #612, #3720, #5027, #7691, #7526, #3763, #2043, #6263, #1878, #4372, #1271, #650, #1920, #3148, #5639, #2540, #6919, #1305, #3796, #6306, #687, #3188, #5684, #63, #2578, #2883, #3584, #6666, #5372, #3540, #3908, #386, #6045, #5417, #4722, #1051, #6429, #6591, #3305, #5811, #7926, #7976, #426, #1008, #3504, #2266, #1659, #193, #4061, #806, #6004, #2918, #967, #2317, #2703, #4763, #5187, #2846, #7292, #7850, #2197, #4810, #5334, #4682, #7334 ),
 .UNSPECIFIED., .F., .F.,
 ( 4, 1, 1, 1, 1, 2, 2, 1, 2, 2, 2, 1, 2, 2, 1, 1, 1, 2, 2, 2, 1, 1, 1, 1, 2, 2, 1, 2, 2, 2, 1, 2, 2, 1, 1, 2, 2, 1, 1, 1, 2, 2, 4 ),
 ( 0.000000000000000000, 0.06250000000000618949, 0.09375000000000655032, 0.1093750000000071193, 0.1171875000000052458, 0.1210937500000043160, 0.1250000000000033862, 0.1562500000000120737, 0.1718750000000147382, 0.1875000000000174027, 0.2500000000000182077, 0.2812500000000194844, 0.2968750000000217049, 0.3125000000000238698, 0.3437500000000262013, 0.3593750000000273670, 0.3671875000000291434, 0.3710937500000290323, 0.3750000000000289213, 0.4999999999999668043, 0.5624999999999343858, 0.5937499999999176215, 0.6093749999999092948, 0.6171874999999059641, 0.6210937499999055200, 0.6249999999999050759, 0.6562499999998950839, 0.6718749999998911981, 0.6874999999998873124, 0.7499999999998724354, 0.7812499999998641087, 0.7968749999998607780, 0.8124999999998574474, 0.8437499999998507860, 0.8593749999998491207, 0.8671874999998483435, 0.8749999999998474554, 0.9062499999998501199, 0.9218749999998540057, 0.9296874999998562261, 0.9335937499998603339, 0.9374999999998643307, 1.000000000000000000 ),
 .UNSPECIFIED. ) ;
#4849 = CC_DESIGN_APPROVAL ( #2517, ( #1419 ) ) ;
#4850 = CARTESIAN_POINT ( 'NONE',  ( -0.3551829056966991915, 2.363969070009024787, -3.041846016155792753 ) ) ;
#4851 = EDGE_CURVE ( 'NONE', #2209, #6986, #18, .T. ) ;
#4852 = CARTESIAN_POINT ( 'NONE',  ( -3.987046614173229475, 3.756917219824143395, 8.267743937948555555 ) ) ;
#4853 = LINE ( 'NONE', #1053, #3050 ) ;
#4854 = CARTESIAN_POINT ( 'NONE',  ( -1.625000000000000222, 2.217843349455980384, -2.674602989331134495 ) ) ;
#4855 = ORIENTED_EDGE ( 'NONE', *, *, #166, .F. ) ;
#4856 = PERSON_AND_ORGANIZATION ( #7862, #8117 ) ;
#4857 = CYLINDRICAL_SURFACE ( 'NONE', #7446, 3.874999999025058539 ) ;
#4858 = PERSON_AND_ORGANIZATION_ROLE ( 'classification_officer' ) ;
#4859 = VERTEX_POINT ( 'NONE', #1963 ) ;
#4860 = CARTESIAN_POINT ( 'NONE',  ( 0.000000000000000000, 3.950000000000000178, -5.108750000000001457 ) ) ;
#4861 = DIRECTION ( 'NONE',  ( 0.000000000000000000, 1.000000000000000000, -0.000000000000000000 ) ) ;
#4862 = DIRECTION ( 'NONE',  ( 1.000000000000000000, 0.000000000000000000, -0.000000000000000000 ) ) ;
#4863 = ORIENTED_EDGE ( 'NONE', *, *, #4976, .F. ) ;
#4864 = CC_DESIGN_PERSON_AND_ORGANIZATION_ASSIGNMENT ( #3604, #4246, ( #1832 ) ) ;
#4865 = CARTESIAN_POINT ( 'NONE',  ( 3.987953385826771946, 4.146499994074615003, 8.231249998505111520 ) ) ;
#4866 = COORDINATED_UNIVERSAL_TIME_OFFSET ( 0, 0, .AHEAD. ) ;
#4867 = ADVANCED_FACE ( 'NONE', ( #1999 ), #5032, .T. ) ;
#4868 = DIRECTION ( 'NONE',  ( -0.000000000000000000, -1.000000000000000000, -0.000000000000000000 ) ) ;
#4869 = ORIENTED_EDGE ( 'NONE', *, *, #8016, .T. ) ;
#4870 = CARTESIAN_POINT ( 'NONE',  ( -4.462046614173229564, 3.753500037802126599, 8.624249954777603477 ) ) ;
#4871 = CARTESIAN_POINT ( 'NONE',  ( 4.470366332363715500, 1.000000000000000888, 2.937534001674282358 ) ) ;
#4872 = COORDINATED_UNIVERSAL_TIME_OFFSET ( 0, 0, .AHEAD. ) ;
#4873 = VERTEX_POINT ( 'NONE', #5074 ) ;
#4874 = CARTESIAN_POINT ( 'NONE',  ( 0.000000000000000000, 5.160877715062512472, 6.858307716807694909 ) ) ;
#4875 = AXIS2_PLACEMENT_3D ( 'NONE', #1739, #5306, #6819 ) ;
#4876 = ORIENTED_EDGE ( 'NONE', *, *, #6123, .F. ) ;
#4877 = EDGE_CURVE ( 'NONE', #5894, #1965, #4456, .T. ) ;
#4878 = FACE_OUTER_BOUND ( 'NONE', #6534, .T. ) ;
#4879 = VECTOR ( 'NONE', #4758, 39.37007874015748143 ) ;
#4880 = AXIS2_PLACEMENT_3D ( 'NONE', #4651, #4032, #6384 ) ;
#4881 = CARTESIAN_POINT ( 'NONE',  ( 2.749999999999999556, 7.521783346412262539, 3.956250000092213615 ) ) ;
#4882 = ADVANCED_FACE ( 'N', ( #738 ), #2621, .T. ) ;
#4883 = APPROVAL_PERSON_ORGANIZATION ( #4726, #1375, #4686 ) ;
#4884 = ORIENTED_EDGE ( 'NONE', *, *, #2865, .F. ) ;
#4885 = CARTESIAN_POINT ( 'NONE',  ( 0.000000000000000000, 2.500000000000000000, 0.000000000000000000 ) ) ;
#4886 = VERTEX_POINT ( 'NONE', #2663 ) ;
#4887 = VECTOR ( 'NONE', #3500, 39.37007874015748143 ) ;
#4888 = VECTOR ( 'NONE', #3454, 39.37007874015748143 ) ;
#4889 = CARTESIAN_POINT ( 'NONE',  ( 3.343750000000001776, 2.500000000000000444, -0.5625000000000001110 ) ) ;
#4890 = CARTESIAN_POINT ( 'NONE',  ( 1.312500000123272725, 4.908106857128372802, -5.108750000000001457 ) ) ;
#4891 = CARTESIAN_POINT ( 'NONE',  ( -3.987046614173228587, 3.753500037802127043, 8.231249998505111520 ) ) ;
#4892 = CIRCLE ( 'NONE', #833, 3.343750000098590913 ) ;
#4893 = CARTESIAN_POINT ( 'NONE',  ( 0.000000000000000000, 1.749999999784896065, 0.000000000000000000 ) ) ;
#4894 = DIRECTION ( 'NONE',  ( 0.000000000000000000, -0.000000000000000000, 1.000000000000000000 ) ) ;
#4895 = EDGE_LOOP ( 'NONE', ( #5124, #2263, #2401, #5938 ) ) ;
#4896 = COORDINATED_UNIVERSAL_TIME_OFFSET ( 0, 0, .AHEAD. ) ;
#4897 = CIRCLE ( 'NONE', #180, 0.3625000012227142521 ) ;
#4898 = DIRECTION ( 'NONE',  ( 0.000000000000000000, -0.000000000000000000, 1.000000000000000000 ) ) ;
#4899 = AXIS2_PLACEMENT_3D ( 'NONE', #5346, #1518, #282 ) ;
#4900 = ORIENTED_EDGE ( 'NONE', *, *, #632, .F. ) ;
#4901 = AXIS2_PLACEMENT_3D ( 'NONE', #4464, #3775, #4343 ) ;
#4902 = DIRECTION ( 'NONE',  ( 0.7071067811865474617, 0.000000000000000000, 0.7071067811865474617 ) ) ;
#4903 = PLANE ( 'NONE',  #587 ) ;
#4904 = FACE_OUTER_BOUND ( 'NONE', #725, .T. ) ;
#4905 = ORIENTED_EDGE ( 'NONE', *, *, #6137, .T. ) ;
#4906 = PERSON_AND_ORGANIZATION ( #7862, #8117 ) ;
#4907 = CARTESIAN_POINT ( 'NONE',  ( 4.067120052493438997, 4.383999996532202736, 9.099249959692768286 ) ) ;
#4908 = AXIS2_PLACEMENT_3D ( 'NONE', #5610, #3654, #6149 ) ;
#4909 = COORDINATED_UNIVERSAL_TIME_OFFSET ( 0, 0, .AHEAD. ) ;
#4910 = LINE ( 'NONE', #6471, #4748 ) ;
#4911 = CARTESIAN_POINT ( 'NONE',  ( 1.624999999811037599, 5.151388682096968097, 2.749999999536767437 ) ) ;
#4912 = AXIS2_PLACEMENT_3D ( 'NONE', #7858, #2732, #2887 ) ;
#4913 = LINE ( 'NONE', #7321, #1093 ) ;
#4914 =( BOUNDED_CURVE ( )  B_SPLINE_CURVE ( 3, ( #5107, #7692, #5071, #1392 ),
 .UNSPECIFIED., .F., .F. ) 
 B_SPLINE_CURVE_WITH_KNOTS ( ( 4, 4 ),
 ( 8.186897041735312450E-13, 0.03375796088403870687 ),
 .UNSPECIFIED. ) 
 CURVE ( )  GEOMETRIC_REPRESENTATION_ITEM ( )  RATIONAL_B_SPLINE_CURVE ( ( 0.5716951606347142611, 0.6501402848013384528, 0.7927633098596811312, 0.9995642358097424074 ) ) 
 REPRESENTATION_ITEM ( '' )  );
#4915 = FACE_BOUND ( 'NONE', #6949, .T. ) ;
#4916 = ORIENTED_EDGE ( 'NONE', *, *, #7320, .F. ) ;
#4917 = LINE ( 'NONE', #1809, #7270 ) ;
#4918 = CARTESIAN_POINT ( 'NONE',  ( 2.815000007187132613, 1.000000000000000222, -3.895000001893597297 ) ) ;
#4919 = PERSON_AND_ORGANIZATION ( #7862, #8117 ) ;
#4920 = ORIENTED_EDGE ( 'NONE', *, *, #7883, .T. ) ;
#4921 = CARTESIAN_POINT ( 'NONE',  ( -2.745000000000000551, 8.719000000000001194, 3.818750000000002753 ) ) ;
#4922 = PRODUCT_DEFINITION ( 'UNKNOWN', '', #4347, #2257 ) ;
#4923 = ORIENTED_EDGE ( 'NONE', *, *, #7929, .T. ) ;
#4924 = CARTESIAN_POINT ( 'NONE',  ( 2.740000000000000657, 7.974000000000001087, 3.823750000000002647 ) ) ;
#4925 = AXIS2_PLACEMENT_3D ( 'NONE', #2894, #5386, #5470 ) ;
#4926 = CARTESIAN_POINT ( 'NONE',  ( 2.749999999999999556, 8.589000000000000412, 4.486250000000000959 ) ) ;
#4927 = EDGE_CURVE ( 'NONE', #1507, #445, #5148, .T. ) ;
#4928 = VERTEX_POINT ( 'NONE', #1881 ) ;
#4929 = CARTESIAN_POINT ( 'NONE',  ( -0.6818077110526901130, 3.637528807515573170, 8.252326836086272266 ) ) ;
#4930 = ORIENTED_EDGE ( 'NONE', *, *, #730, .T. ) ;
#4931 = DIRECTION ( 'NONE',  ( -0.000000000000000000, 1.000000000000000000, -0.000000000000000000 ) ) ;
#4932 = DIRECTION ( 'NONE',  ( 1.000000000000000000, 0.000000000000000000, 0.000000000000000000 ) ) ;
#4933 = CARTESIAN_POINT ( 'NONE',  ( 2.740000000000000657, 7.964000000000000412, 3.823750000000002647 ) ) ;
#4934 = CARTESIAN_POINT ( 'NONE',  ( 0.000000000000000000, 0.000000000000000000, 3.823750000000002647 ) ) ;
#4935 = ORIENTED_EDGE ( 'NONE', *, *, #6201, .F. ) ;
#4936 = PERSON_AND_ORGANIZATION_ROLE ( 'design_owner' ) ;
#4937 = CARTESIAN_POINT ( 'NONE',  ( 0.000000000000000000, 3.950000000000000178, 6.956250000000000711 ) ) ;
#4938 = DIRECTION ( 'NONE',  ( -0.000000000000000000, -1.000000000000000000, -0.000000000000000000 ) ) ;
#4939 = CARTESIAN_POINT ( 'NONE',  ( 2.750000000000000444, 7.964000000000000412, 4.323750000000001315 ) ) ;
#4940 = ADVANCED_FACE ( 'NONE', ( #810 ), #3310, .F. ) ;
#4941 = EDGE_LOOP ( 'NONE', ( #4509, #3435, #4033, #5105 ) ) ;
#4942 = ADVANCED_FACE ( 'NONE', ( #3518 ), #4501, .T. ) ;
#4943 = APPROVAL_ROLE ( '' ) ;
#4944 = LINE ( 'NONE', #4327, #7558 ) ;
#4945 = DATE_AND_TIME ( #6952, #7278 ) ;
#4946 = CARTESIAN_POINT ( 'NONE',  ( -2.740000000000000213, 8.729000000000002757, 3.813750000000002416 ) ) ;
#4947 = CC_DESIGN_SECURITY_CLASSIFICATION ( #7597, ( #2206 ) ) ;
#4948 = CARTESIAN_POINT ( 'NONE',  ( -1.201750000000000318, 5.151750000000000718, 6.956250000000000711 ) ) ;
#4949 = PLANE ( 'NONE',  #7846 ) ;
#4950 = DIRECTION ( 'NONE',  ( -0.000000000000000000, 1.000000000000000000, 0.000000000000000000 ) ) ;
#4951 = ORIENTED_EDGE ( 'NONE', *, *, #2446, .T. ) ;
#4952 = CARTESIAN_POINT ( 'NONE',  ( -0.7431911064911158604, 4.051321384912569101, 7.935451190925254750 ) ) ;
#4953 = EDGE_CURVE ( 'NONE', #7021, #2549, #6992, .T. ) ;
#4954 = DIRECTION ( 'NONE',  ( 0.000000000000000000, 0.000000000000000000, 1.000000000000000000 ) ) ;
#4955 = DIRECTION ( 'NONE',  ( -1.000000000000000000, -0.000000000000000000, -0.000000000000000000 ) ) ;
#4956 = APPROVAL_ROLE ( '' ) ;
#4957 = CARTESIAN_POINT ( 'NONE',  ( 2.750000000000003109, 8.588999999999998636, 2.411250000000000782 ) ) ;
#4958 = ORIENTED_EDGE ( 'NONE', *, *, #6044, .T. ) ;
#4959 = LINE ( 'NONE', #7499, #7592 ) ;
#4960 = ORIENTED_EDGE ( 'NONE', *, *, #6650, .T. ) ;
#4961 = DIRECTION ( 'NONE',  ( -0.000000000000000000, -1.000000000000000000, -0.000000000000000000 ) ) ;
#4962 = EDGE_LOOP ( 'NONE', ( #554, #7033, #1075, #6697 ) ) ;
#4963 = CC_DESIGN_PERSON_AND_ORGANIZATION_ASSIGNMENT ( #294, #2834, ( #3521 ) ) ;
#4964 = ORIENTED_EDGE ( 'NONE', *, *, #5601, .T. ) ;
#4965 = PERSON ( 'NAUO-PER5', 'UNSPECIFIED', 'UNSPECIFIED', ('UNSPECIFIED'), ('UNSPECIFIED'), ('UNSPECIFIED') ) ;
#4966 = EDGE_CURVE ( 'NONE', #6623, #4491, #4615, .T. ) ;
#4967 = CARTESIAN_POINT ( 'NONE',  ( 4.462953385826772035, 3.753500037802128375, 8.231249998505111520 ) ) ;
#4968 = DIRECTION ( 'NONE',  ( -0.000000000000000000, -0.000000000000000000, 1.000000000000000000 ) ) ;
#4969 = CARTESIAN_POINT ( 'NONE',  ( 1.039062322834645835, 2.913002440944882476, -4.272368937007874123 ) ) ;
#4970 = CARTESIAN_POINT ( 'NONE',  ( -2.750000000000000444, 8.729000000000002757, 4.313750000000002416 ) ) ;
#4971 = ORIENTED_EDGE ( 'NONE', *, *, #2192, .F. ) ;
#4972 = MECHANICAL_CONTEXT ( 'NONE', #7363, 'mechanical' ) ;
#4973 = APPROVAL_PERSON_ORGANIZATION ( #1551, #2066, #3991 ) ;
#4974 = DIRECTION ( 'NONE',  ( 0.7071067811865474617, -0.7071067811865474617, 0.000000000000000000 ) ) ;
#4975 = EDGE_LOOP ( 'NONE', ( #5985, #5353, #6166, #3067, #1121, #4345, #3766, #4263 ) ) ;
#4976 = EDGE_CURVE ( 'NONE', #417, #6003, #1600, .T. ) ;
#4977 = EDGE_CURVE ( 'NONE', #1793, #3439, #3404, .T. ) ;
#4978 = CARTESIAN_POINT ( 'NONE',  ( 0.000000000000000000, 3.001975734461090560E-16, -2.845000000000001528 ) ) ;
#4979 = DIRECTION ( 'NONE',  ( 1.000000000000000000, 0.000000000000000000, -0.000000000000000000 ) ) ;
#4980 = CARTESIAN_POINT ( 'NONE',  ( 1.625000000000000222, 2.217843350849094897, 2.674602988580442542 ) ) ;
#4981 = VERTEX_POINT ( 'NONE', #3356 ) ;
#4982 = CALENDAR_DATE ( 2026, 8, 10 ) ;
#4983 = EDGE_CURVE ( 'NONE', #8139, #3899, #2822, .T. ) ;
#4984 = CARTESIAN_POINT ( 'NONE',  ( 4.462953385826772923, 4.225666661560477877, 8.782583289749322120 ) ) ;
#4985 = CALENDAR_DATE ( 2026, 8, 10 ) ;
#4986 = CARTESIAN_POINT ( 'NONE',  ( 2.750000000000003109, 7.339000000000001300, 3.471636850393700513 ) ) ;
#4987 = CARTESIAN_POINT ( 'NONE',  ( -3.987046614173228587, 3.753500037802127043, 8.231249998505111520 ) ) ;
#4988 = PLANE ( 'NONE',  #2315 ) ;
#4989 = CARTESIAN_POINT ( 'NONE',  ( -1.312500000000000444, 7.352492870354978116, 3.316250000370396744 ) ) ;
#4990 = EDGE_LOOP ( 'NONE', ( #7768, #664, #6503, #2386 ) ) ;
#4991 = CARTESIAN_POINT ( 'NONE',  ( -3.987046614173229031, 4.225666661560476989, 8.782583289749323896 ) ) ;
#4992 = EDGE_CURVE ( 'NONE', #7024, #3656, #2292, .T. ) ;
#4993 = CARTESIAN_POINT ( 'NONE',  ( -1.624999999999999778, 3.950000000000000178, -5.108750000000001457 ) ) ;
#4994 = PLANE ( 'NONE',  #5457 ) ;
#4995 = COORDINATED_UNIVERSAL_TIME_OFFSET ( 0, 0, .AHEAD. ) ;
#4996 = VERTEX_POINT ( 'NONE', #5308 ) ;
#4997 = FACE_OUTER_BOUND ( 'NONE', #6788, .T. ) ;
#4998 = ADVANCED_FACE ( 'NONE', ( #7089 ), #4002, .F. ) ;
#4999 = DIRECTION ( 'NONE',  ( -1.000000000000000000, 0.000000000000000000, -0.000000000000000000 ) ) ;
#5000 = CIRCLE ( 'NONE', #14, 1.624999999999999778 ) ;
#5001 = VERTEX_POINT ( 'NONE', #1473 ) ;
#5002 = EDGE_LOOP ( 'NONE', ( #917, #4507, #1708, #6550 ) ) ;
#5003 = AXIS2_PLACEMENT_3D ( 'NONE', #2984, #5481, #8042 ) ;
#5004 = LOCAL_TIME ( 0, 37, 23.00000000000000000, #3825 ) ;
#5005 = DIRECTION ( 'NONE',  ( -1.000000000000000000, 0.000000000000000000, -0.000000000000000000 ) ) ;
#5006 = CARTESIAN_POINT ( 'NONE',  ( 1.177243228188373791, 3.368106800967091807, -5.108749999999999680 ) ) ;
#5007 = DIRECTION ( 'NONE',  ( -0.000000000000000000, -1.000000000000000000, -0.000000000000000000 ) ) ;
#5008 = ORIENTED_EDGE ( 'NONE', *, *, #4822, .T. ) ;
#5009 = PERSON_AND_ORGANIZATION_ROLE ( 'classification_officer' ) ;
#5010 = DIRECTION ( 'NONE',  ( -0.1218497812680350983, 0.000000000000000000, 0.9925485533740563415 ) ) ;
#5011 = CARTESIAN_POINT ( 'NONE',  ( -0.7417920657368231030, 3.838932697565026864, 8.523525407967506240 ) ) ;
#5012 = EDGE_LOOP ( 'NONE', ( #2369, #3081, #1799, #6051 ) ) ;
#5013 = CIRCLE ( 'NONE', #4223, 1.624999999999999778 ) ;
#5014 = CC_DESIGN_DATE_AND_TIME_ASSIGNMENT ( #4326, #681, ( #1622 ) ) ;
#5015 = AXIS2_PLACEMENT_3D ( 'NONE', #7224, #4670, #6490 ) ;
#5016 = CARTESIAN_POINT ( 'NONE',  ( -2.946793808642157231, 2.500000000130568889, -0.5624999991015005030 ) ) ;
#5017 = VERTEX_POINT ( 'NONE', #6608 ) ;
#5018 = SECURITY_CLASSIFICATION_LEVEL ( 'unclassified' ) ;
#5019 = DIRECTION ( 'NONE',  ( 0.000000000000000000, 0.000000000000000000, 1.000000000000000000 ) ) ;
#5020 = DATE_AND_TIME ( #4449, #5034 ) ;
#5021 = DIRECTION ( 'NONE',  ( 0.000000000000000000, 0.7071067811865474617, -0.7071067811865474617 ) ) ;
#5022 = CARTESIAN_POINT ( 'NONE',  ( -0.7499999999999993339, 3.950000000000000178, 7.231250000000000178 ) ) ;
#5023 = EDGE_CURVE ( 'NONE', #1962, #3236, #6865, .T. ) ;
#5024 = AXIS2_PLACEMENT_3D ( 'NONE', #6971, #2592, #5084 ) ;
#5025 = CC_DESIGN_APPROVAL ( #2217, ( #1242 ) ) ;
#5026 = EDGE_CURVE ( 'NONE', #7925, #1938, #7257, .T. ) ;
#5027 = CARTESIAN_POINT ( 'NONE',  ( -3.987046614173229475, 3.760254621899925542, 8.179444766282907509 ) ) ;
#5028 = DIRECTION ( 'NONE',  ( 1.000000000000000000, -1.681137231067760553E-15, 0.000000000000000000 ) ) ;
#5029 = AXIS2_PLACEMENT_3D ( 'NONE', #4458, #4582, #3802 ) ;
#5030 = DIRECTION ( 'NONE',  ( 0.000000000000000000, -1.000000000000000000, 0.000000000000000000 ) ) ;
#5031 = VERTEX_POINT ( 'NONE', #2859 ) ;
#5032 = PLANE ( 'NONE',  #980 ) ;
#5033 =( LENGTH_UNIT ( ) NAMED_UNIT ( * ) SI_UNIT ( $, .METRE. ) );
#5034 = LOCAL_TIME ( 0, 37, 23.00000000000000000, #5726 ) ;
#5035 = CARTESIAN_POINT ( 'NONE',  ( -1.187499999999999778, 4.553161336648244628, 6.294740251547498389 ) ) ;
#5036 = APPROVAL_ROLE ( '' ) ;
#5037 = ORIENTED_EDGE ( 'NONE', *, *, #589, .T. ) ;
#5038 = CARTESIAN_POINT ( 'NONE',  ( 2.740000000000001545, 8.719000000000002970, 4.323750000000001315 ) ) ;
#5039 = APPROVAL_PERSON_ORGANIZATION ( #1178, #5621, #4290 ) ;
#5040 = CARTESIAN_POINT ( 'NONE',  ( -2.875000000000000888, 1.000000000000000222, -2.975000000000000977 ) ) ;
#5041 = CARTESIAN_POINT ( 'NONE',  ( -1.312500000000000444, 7.352492870354978116, 3.316250000000001474 ) ) ;
#5042 = LINE ( 'NONE', #7019, #4237 ) ;
#5043 = VECTOR ( 'NONE', #1206, 39.37007874015748854 ) ;
#5044 = ADVANCED_FACE ( 'NONE', ( #7129 ), #4116, .T. ) ;
#5045 = VERTEX_POINT ( 'NONE', #6528 ) ;
#5046 = ORIENTED_EDGE ( 'NONE', *, *, #5026, .T. ) ;
#5047 = AXIS2_PLACEMENT_3D ( 'NONE', #4695, #983, #5976 ) ;
#5048 = CARTESIAN_POINT ( 'NONE',  ( 3.987953385826772390, 3.754593536049173341, 8.207305520649800457 ) ) ;
#5049 = CARTESIAN_POINT ( 'NONE',  ( 0.6955817875586080001, 5.063844427419111227, -5.108750000000004121 ) ) ;
#5050 = FACE_OUTER_BOUND ( 'NONE', #7571, .T. ) ;
#5051 = ORIENTED_EDGE ( 'NONE', *, *, #7579, .F. ) ;
#5052 = PERSON ( 'NAUO-PER8', 'UNSPECIFIED', 'UNSPECIFIED', ('UNSPECIFIED'), ('UNSPECIFIED'), ('UNSPECIFIED') ) ;
#5053 = CALENDAR_DATE ( 2026, 8, 10 ) ;
#5054 = CARTESIAN_POINT ( 'NONE',  ( 3.987953385826771946, 3.766169374065351239, 8.300671349344955985 ) ) ;
#5055 = AXIS2_PLACEMENT_3D ( 'NONE', #4435, #1860, #7514 ) ;
#5056 = VECTOR ( 'NONE', #2613, 39.37007874015748143 ) ;
#5057 = ORIENTED_EDGE ( 'NONE', *, *, #1550, .F. ) ;
#5058 = AXIS2_PLACEMENT_3D ( 'NONE', #1027, #6020, #405 ) ;
#5059 = CARTESIAN_POINT ( 'NONE',  ( 0.000000000000000000, 1.749999999784895843, 0.000000000000000000 ) ) ;
#5060 = CARTESIAN_POINT ( 'NONE',  ( -2.749999999999998668, 7.338999999999999524, 3.471636850393700513 ) ) ;
#5061 = DIRECTION ( 'NONE',  ( 0.9531066744677130220, 0.000000000000000000, 0.3026345437736693289 ) ) ;
#5062 = VERTEX_POINT ( 'NONE', #2776 ) ;
#5063 = PERSON_AND_ORGANIZATION_ROLE ( 'design_supplier' ) ;
#5064 = CARTESIAN_POINT ( 'NONE',  ( -3.796513189164426816, 1.000000000000000888, -2.946478859991635169 ) ) ;
#5065 = PERSON_AND_ORGANIZATION_ROLE ( 'classification_officer' ) ;
#5066 = CC_DESIGN_PERSON_AND_ORGANIZATION_ASSIGNMENT ( #6785, #3005, ( #5310 ) ) ;
#5067 = CARTESIAN_POINT ( 'NONE',  ( 3.179822820549663476, 2.000074506952454811, 0.5624999982029994516 ) ) ;
#5068 = DIRECTION ( 'NONE',  ( -0.000000000000000000, 0.7071067811865474617, 0.7071067811865474617 ) ) ;
#5069 = ADVANCED_FACE ( 'NONE', ( #7820 ), #2876, .T. ) ;
#5070 = DIRECTION ( 'NONE',  ( 0.000000000000000000, 0.000000000000000000, 1.000000000000000000 ) ) ;
#5071 = CARTESIAN_POINT ( 'NONE',  ( -0.4139007109890988079, 5.536672282146934521, 4.083473622047245399 ) ) ;
#5072 = FACE_OUTER_BOUND ( 'NONE', #2236, .T. ) ;
#5073 = EDGE_LOOP ( 'NONE', ( #4720, #6699, #3393, #3229 ) ) ;
#5074 = CARTESIAN_POINT ( 'NONE',  ( 2.815000007187131725, 1.365923996832131609E-16, -3.895000001893597741 ) ) ;
#5075 = SHAPE_REPRESENTATION_RELATIONSHIP ( 'NONE' , 'NONE' ,  #6040, #1241 ) ;
#5076 = FACE_BOUND ( 'NONE', #4602, .T. ) ;
#5077 = B_SPLINE_CURVE_WITH_KNOTS ( 'NONE', 3,
 ( #2268, #268, #1586, #7804, #3465, #5965, #4766, #7294, #1663, #4515, #3249, #123 ),
 .UNSPECIFIED., .F., .F.,
 ( 4, 2, 2, 2, 2, 4 ),
 ( 8.673617379884035472E-18, 0.004953213565686583227, 0.009906427131373157779, 0.01238303391421645416, 0.01485964069705974881, 0.01981285426274633638 ),
 .UNSPECIFIED. ) ;
#5078 = APPROVAL_DATE_TIME ( #69, #4565 ) ;
#5079 =( BOUNDED_CURVE ( )  B_SPLINE_CURVE ( 3, ( #6804, #7403, #8090, #3613 ),
 .UNSPECIFIED., .F., .F. ) 
 B_SPLINE_CURVE_WITH_KNOTS ( ( 4, 4 ),
 ( 0.000000000000000000, 0.01230154035705741285 ),
 .UNSPECIFIED. ) 
 CURVE ( )  GEOMETRIC_REPRESENTATION_ITEM ( )  RATIONAL_B_SPLINE_CURVE ( ( 0.5972799528396778301, 0.5865781935274074765, 0.5767594089368136556, 0.5678235990678964784 ) ) 
 REPRESENTATION_ITEM ( '' )  );
#5080 = ORIENTED_EDGE ( 'NONE', *, *, #4588, .F. ) ;
#5081 = CARTESIAN_POINT ( 'NONE',  ( 2.537499998660271761, 3.550000000000001155, 2.790532913385826763 ) ) ;
#5082 = ADVANCED_FACE ( 'N', ( #4824 ), #4903, .T. ) ;
#5083 = EDGE_CURVE ( 'NONE', #3210, #3600, #3200, .T. ) ;
#5084 = DIRECTION ( 'NONE',  ( -1.000000000000000000, 0.000000000000000000, 0.000000000000000000 ) ) ;
#5085 = CYLINDRICAL_SURFACE ( 'NONE', #4901, 0.7499999999999993339 ) ;
#5086 = CARTESIAN_POINT ( 'NONE',  ( 2.750000000000000888, 8.729000000000002757, 3.333750000000001990 ) ) ;
#5087 = ORIENTED_EDGE ( 'NONE', *, *, #2525, .T. ) ;
#5088 = ADVANCED_FACE ( 'N', ( #5509 ), #5553, .T. ) ;
#5089 = ORIENTED_EDGE ( 'NONE', *, *, #2493, .F. ) ;
#5090 = CARTESIAN_POINT ( 'NONE',  ( 3.987953385826771946, 3.757384381775243920, 8.192364704391765784 ) ) ;
#5091 = CARTESIAN_POINT ( 'NONE',  ( 1.304290195953534237, 4.098156632275986588, -5.108750000000004121 ) ) ;
#5092 = CARTESIAN_POINT ( 'NONE',  ( 3.987953385826772834, 3.815844187783016483, 8.374988138248586012 ) ) ;
#5093 = EDGE_CURVE ( 'NONE', #7410, #3177, #8120, .T. ) ;
#5094 = ORIENTED_EDGE ( 'NONE', *, *, #7384, .T. ) ;
#5095 = EDGE_CURVE ( 'NONE', #2223, #2302, #6098, .T. ) ;
#5096 = DIRECTION ( 'NONE',  ( 0.000000000000000000, 1.000000000000000000, 0.000000000000000000 ) ) ;
#5097 = CARTESIAN_POINT ( 'NONE',  ( -2.375000000000003109, 2.762499999999999289, 6.956249999999992717 ) ) ;
#5098 = VERTEX_POINT ( 'NONE', #7482 ) ;
#5099 = SECURITY_CLASSIFICATION ( '', '', #3558 ) ;
#5100 = APPLICATION_PROTOCOL_DEFINITION ( 'international standard', 'config_control_design', 1994, #7415 ) ;
#5101 = PLANE ( 'NONE',  #7838 ) ;
#5102 = DATE_TIME_ROLE ( 'classification_date' ) ;
#5103 = DIRECTION ( 'NONE',  ( 0.000000000000000000, 0.000000000000000000, 1.000000000000000000 ) ) ;
#5104 = CC_DESIGN_APPROVAL ( #4313, ( #3413 ) ) ;
#5105 = ORIENTED_EDGE ( 'NONE', *, *, #2192, .T. ) ;
#5106 = CARTESIAN_POINT ( 'NONE',  ( 3.651126734928074491, 1.365923996832131609E-16, -1.298036420927624501 ) ) ;
#5107 = CARTESIAN_POINT ( 'NONE',  ( -1.187499999443275334, 5.002317768720649482, 4.083473622047245399 ) ) ;
#5108 = CC_DESIGN_PERSON_AND_ORGANIZATION_ASSIGNMENT ( #4662, #5937, ( #1164 ) ) ;
#5109 = CARTESIAN_POINT ( 'NONE',  ( -3.343750000000002220, 2.500000000000000444, 0.5625000000000003331 ) ) ;
#5110 = ORIENTED_EDGE ( 'NONE', *, *, #8176, .T. ) ;
#5111 = DIRECTION ( 'NONE',  ( 0.000000000000000000, 0.000000000000000000, 1.000000000000000000 ) ) ;
#5112 = LINE ( 'NONE', #6054, #6367 ) ;
#5113 = APPROVAL_PERSON_ORGANIZATION ( #3110, #2217, #2534 ) ;
#5114 = ORIENTED_EDGE ( 'NONE', *, *, #7643, .T. ) ;
#5115 = DIRECTION ( 'NONE',  ( 1.000000000000000000, 0.000000000000000000, 0.000000000000000000 ) ) ;
#5116 = DIRECTION ( 'NONE',  ( -0.000000000000000000, -0.7071067811865474617, -0.7071067811865474617 ) ) ;
#5117 = APPROVAL_ROLE ( '' ) ;
#5118 = ORIENTED_EDGE ( 'NONE', *, *, #216, .F. ) ;
#5119 = ADVANCED_FACE ( 'NONE', ( #8071 ), #1829, .F. ) ;
#5120 = APPROVAL ( #3260, 'UNSPECIFIED' ) ;
#5121 = CARTESIAN_POINT ( 'NONE',  ( 2.740000000000001545, 7.973999999999999311, 4.323750000000001315 ) ) ;
#5122 = LINE ( 'NONE', #2011, #2422 ) ;
#5123 = VERTEX_POINT ( 'NONE', #1099 ) ;
#5124 = ORIENTED_EDGE ( 'NONE', *, *, #4168, .F. ) ;
#5125 = ADVANCED_FACE ( 'NONE', ( #3712 ), #1753, .T. ) ;
#5126 = CARTESIAN_POINT ( 'NONE',  ( 3.987953385826772834, 3.757861515926419482, 8.190024801382651987 ) ) ;
#5127 = CARTESIAN_POINT ( 'NONE',  ( 1.102289196576730079, 3.237202587873624360, -5.108750000000004121 ) ) ;
#5128 = CARTESIAN_POINT ( 'NONE',  ( 2.875000000000000888, -3.820994292482255198E-18, -2.975000000000000977 ) ) ;
#5129 = FACE_OUTER_BOUND ( 'NONE', #5388, .T. ) ;
#5130 = VERTEX_POINT ( 'NONE', #8031 ) ;
#5131 = LOCAL_TIME ( 0, 37, 23.00000000000000000, #2077 ) ;
#5132 = CARTESIAN_POINT ( 'NONE',  ( 1.312500000000000444, 5.969165905511811587, 3.161250000000001670 ) ) ;
#5133 = CARTESIAN_POINT ( 'NONE',  ( 4.462953385826771147, 3.753500037801649203, 7.838250042231665660 ) ) ;
#5134 = ORIENTED_EDGE ( 'NONE', *, *, #3657, .F. ) ;
#5135 = PERSON_AND_ORGANIZATION ( #7862, #8117 ) ;
#5136 = VECTOR ( 'NONE', #2481, 39.37007874015748143 ) ;
#5137 = CARTESIAN_POINT ( 'NONE',  ( 0.000000000000000000, 3.950000000000000178, 3.691250000234376660 ) ) ;
#5138 = CC_DESIGN_APPROVAL ( #4714, ( #4483 ) ) ;
#5139 = CARTESIAN_POINT ( 'NONE',  ( 0.7335374419612976649, 3.792759758930657199, 7.960425892670179415 ) ) ;
#5140 = CARTESIAN_POINT ( 'NONE',  ( 0.7499999999999993339, 3.950000000000000178, 8.543750000000002842 ) ) ;
#5141 = CIRCLE ( 'NONE', #7121, 0.7499999999999993339 ) ;
#5142 = ORIENTED_EDGE ( 'NONE', *, *, #3732, .T. ) ;
#5143 = APPROVAL_PERSON_ORGANIZATION ( #4746, #6544, #868 ) ;
#5144 = CARTESIAN_POINT ( 'NONE',  ( -2.946793808531571468, 2.500000000000000000, 0.5625000000000002220 ) ) ;
#5145 = LINE ( 'NONE', #2618, #6640 ) ;
#5146 = CARTESIAN_POINT ( 'NONE',  ( -3.987046614173229919, 4.134652525424356462, 8.298484949317895598 ) ) ;
#5147 = EDGE_LOOP ( 'NONE', ( #3191, #5619, #2866, #3776, #7210 ) ) ;
#5148 = LINE ( 'NONE', #7696, #1107 ) ;
#5149 = ORIENTED_EDGE ( 'NONE', *, *, #7167, .F. ) ;
#5150 = CARTESIAN_POINT ( 'NONE',  ( 1.406273820872128821, 2.812660052342379036, 7.277379520629165377 ) ) ;
#5151 = CARTESIAN_POINT ( 'NONE',  ( 0.000000000000000000, 5.113999999999999879, 0.000000000000000000 ) ) ;
#5152 = DIRECTION ( 'NONE',  ( 0.000000000000000000, 0.000000000000000000, 1.000000000000000000 ) ) ;
#5153 = APPROVAL_ROLE ( '' ) ;
#5154 = VERTEX_POINT ( 'NONE', #4156 ) ;
#5155 = VECTOR ( 'NONE', #2058, 39.37007874015748143 ) ;
#5156 = CIRCLE ( 'NONE', #7827, 0.3625000000000019318 ) ;
#5157 = ADVANCED_FACE ( 'NONE', ( #1061 ), #6209, .T. ) ;
#5158 = AXIS2_PLACEMENT_3D ( 'NONE', #7010, #4498, #5115 ) ;
#5159 = CARTESIAN_POINT ( 'NONE',  ( 1.500000000000000444, 5.113999999999999879, -2.750000000000000444 ) ) ;
#5160 = CARTESIAN_POINT ( 'NONE',  ( -2.750000000000000444, 8.719000000000002970, 3.833750000000001545 ) ) ;
#5161 = EDGE_LOOP ( 'NONE', ( #2781, #2389 ) ) ;
#5162 = CIRCLE ( 'NONE', #5029, 0.7499999999999993339 ) ;
#5163 = VERTEX_POINT ( 'NONE', #4196 ) ;
#5164 = CIRCLE ( 'NONE', #4111, 3.000000000065115024 ) ;
#5165 = APPROVAL ( #6357, 'UNSPECIFIED' ) ;
#5166 = LOCAL_TIME ( 0, 37, 23.00000000000000000, #5888 ) ;
#5167 = SECURITY_CLASSIFICATION ( '', '', #6342 ) ;
#5168 = PERSON ( 'NAUO-PER10', 'UNSPECIFIED', 'UNSPECIFIED', ('UNSPECIFIED'), ('UNSPECIFIED'), ('UNSPECIFIED') ) ;
#5169 = CARTESIAN_POINT ( 'NONE',  ( 3.987953385826772390, 4.043411590721873061, 8.058147833246822600 ) ) ;
#5170 = FACE_OUTER_BOUND ( 'NONE', #8028, .T. ) ;
#5171 =( BOUNDED_CURVE ( )  B_SPLINE_CURVE ( 3, ( #1149, #3607, #6107, #527 ),
 .UNSPECIFIED., .F., .T. ) 
 B_SPLINE_CURVE_WITH_KNOTS ( ( 4, 4 ),
 ( 0.000000000000000000, 0.01230154035705745275 ),
 .UNSPECIFIED. ) 
 CURVE ( )  GEOMETRIC_REPRESENTATION_ITEM ( )  RATIONAL_B_SPLINE_CURVE ( ( 0.5678235990678963674, 0.5767594089368156540, 0.5865781935274119174, 0.5972799528396851576 ) ) 
 REPRESENTATION_ITEM ( '' )  );
#5172 = FACE_OUTER_BOUND ( 'NONE', #6114, .T. ) ;
#5173 = CARTESIAN_POINT ( 'NONE',  ( 3.987953385826774166, 4.054690900397992515, 8.397573164612390784 ) ) ;
#5174 = EDGE_LOOP ( 'NONE', ( #3697, #7644, #3091, #6446 ) ) ;
#5175 = VECTOR ( 'NONE', #7843, 39.37007874015748854 ) ;
#5176 = CARTESIAN_POINT ( 'NONE',  ( -3.651126736044647547, 1.365923996832131609E-16, -1.298036422709905713 ) ) ;
#5177 = FACE_OUTER_BOUND ( 'NONE', #396, .T. ) ;
#5178 = ORIENTED_EDGE ( 'NONE', *, *, #6929, .F. ) ;
#5179 = AXIS2_PLACEMENT_3D ( 'NONE', #2809, #2318, #5916 ) ;
#5180 = CALENDAR_DATE ( 2026, 8, 10 ) ;
#5181 = CARTESIAN_POINT ( 'NONE',  ( 4.462953385826771147, 4.146499994074615003, 8.231249998505111520 ) ) ;
#5182 = DIRECTION ( 'NONE',  ( 0.000000000000000000, 0.000000000000000000, -1.000000000000000000 ) ) ;
#5183 = DIRECTION ( 'NONE',  ( 0.000000000000000000, 0.000000000000000000, 1.000000000000000000 ) ) ;
#5184 = EDGE_CURVE ( 'NONE', #1434, #1186, #630, .T. ) ;
#5185 = CIRCLE ( 'NONE', #6241, 0.3625000012227142521 ) ;
#5186 = ORIENTED_EDGE ( 'NONE', *, *, #5840, .T. ) ;
#5187 = CARTESIAN_POINT ( 'NONE',  ( -3.987046614173228143, 4.138119654530659552, 8.173848920212014590 ) ) ;
#5188 = CARTESIAN_POINT ( 'NONE',  ( 0.000000000000000000, 3.950000000000000178, 2.750000000234376074 ) ) ;
#5189 = CARTESIAN_POINT ( 'NONE',  ( -3.987046614173229475, 3.974973691465472747, 8.427747322941382180 ) ) ;
#5190 = ORIENTED_EDGE ( 'NONE', *, *, #731, .T. ) ;
#5191 = CARTESIAN_POINT ( 'NONE',  ( 0.000000000000000000, 2.875000000000000444, 3.742515787401575533 ) ) ;
#5192 =( LENGTH_UNIT ( ) NAMED_UNIT ( * ) SI_UNIT ( $, .METRE. ) );
#5193 = LINE ( 'NONE', #1311, #3333 ) ;
#5194 = DATE_AND_TIME ( #2710, #6669 ) ;
#5195 = VECTOR ( 'NONE', #7919, 39.37007874015748854 ) ;
#5196 = VERTEX_POINT ( 'NONE', #3864 ) ;
#5197 = DIRECTION ( 'NONE',  ( 0.000000000000000000, -0.000000000000000000, -1.000000000000000000 ) ) ;
#5198 = EDGE_CURVE ( 'NONE', #6635, #2954, #4478, .T. ) ;
#5199 = CARTESIAN_POINT ( 'NONE',  ( -1.625000000000000222, 5.639000000000001123, 0.1249999999999997641 ) ) ;
#5200 = CC_DESIGN_APPROVAL ( #4358, ( #4146 ) ) ;
#5201 = DIRECTION ( 'NONE',  ( 0.000000000000000000, 0.000000000000000000, 1.000000000000000000 ) ) ;
#5202 = ORIENTED_EDGE ( 'NONE', *, *, #4126, .T. ) ;
#5203 = DATE_AND_TIME ( #7917, #3711 ) ;
#5204 = ORIENTED_EDGE ( 'NONE', *, *, #3039, .T. ) ;
#5205 = ADVANCED_FACE ( 'NONE', ( #1864 ), #2831, .T. ) ;
#5206 = DIRECTION ( 'NONE',  ( 0.000000000000000000, 0.000000000000000000, -1.000000000000000000 ) ) ;
#5207 = CARTESIAN_POINT ( 'NONE',  ( 3.987953385826772390, 3.753500037802127931, 8.219224099256663862 ) ) ;
#5208 = APPROVAL ( #7565, 'UNKNOWN' ) ;
#5209 = CARTESIAN_POINT ( 'NONE',  ( 4.462953385826771147, 3.753500037802127931, 7.838250042232624892 ) ) ;
#5210 = CARTESIAN_POINT ( 'NONE',  ( 3.987953385826772390, 3.866991449159138394, 8.409411560744331382 ) ) ;
#5211 = ORIENTED_EDGE ( 'NONE', *, *, #5849, .T. ) ;
#5212 = PRODUCT ( 'bench vise6-', 'bench vise6-', '', ( #6514 ) ) ;
#5213 = DIRECTION ( 'NONE',  ( 0.000000000000000000, -1.000000000000000000, 0.000000000000000000 ) ) ;
#5214 = CARTESIAN_POINT ( 'NONE',  ( -2.749999999999999556, 8.589000000000000412, 3.243476614173228967 ) ) ;
#5215 = ORIENTED_EDGE ( 'NONE', *, *, #7720, .F. ) ;
#5216 = COORDINATED_UNIVERSAL_TIME_OFFSET ( 0, 0, .AHEAD. ) ;
#5217 = DIRECTION ( 'NONE',  ( -0.000000000000000000, 0.000000000000000000, -1.000000000000000000 ) ) ;
#5218 = COORDINATED_UNIVERSAL_TIME_OFFSET ( 0, 0, .AHEAD. ) ;
#5219 = PLANE ( 'NONE',  #7942 ) ;
#5220 = CARTESIAN_POINT ( 'NONE',  ( -0.7499999999999993339, 3.950000000000000178, 7.918749999999998401 ) ) ;
#5221 = ADVANCED_FACE ( 'NONE', ( #1987 ), #6994, .F. ) ;
#5222 = VERTEX_POINT ( 'NONE', #8161 ) ;
#5223 = CARTESIAN_POINT ( 'NONE',  ( 0.000000000000000000, 3.950000000000000178, -4.308749999765625560 ) ) ;
#5224 = EDGE_CURVE ( 'NONE', #1117, #442, #3919, .T. ) ;
#5225 = CARTESIAN_POINT ( 'NONE',  ( -3.987046614173229475, 4.107055349781922438, 8.350119983547221736 ) ) ;
#5226 = VERTEX_POINT ( 'NONE', #4406 ) ;
#5227 = CARTESIAN_POINT ( 'NONE',  ( 1.624999999999999556, 2.076218724953421191, -2.749999999536766992 ) ) ;
#5228 = DIRECTION ( 'NONE',  ( -0.6838295180757010261, -0.7296417229374689839, 0.0003825665906705778070 ) ) ;
#5229 = DIRECTION ( 'NONE',  ( 0.000000000000000000, 0.000000000000000000, -1.000000000000000000 ) ) ;
#5230 = LINE ( 'NONE', #6356, #6888 ) ;
#5231 = SECURITY_CLASSIFICATION_LEVEL ( 'unclassified' ) ;
#5232 = VERTEX_POINT ( 'NONE', #6911 ) ;
#5233 = CARTESIAN_POINT ( 'NONE',  ( -1.624999999371729231, 2.076218724780642511, 2.750000000000000444 ) ) ;
#5234 = DIRECTION ( 'NONE',  ( 0.000000000000000000, 0.000000000000000000, 1.000000000000000000 ) ) ;
#5235 = PLANE ( 'NONE',  #34 ) ;
#5236 = CARTESIAN_POINT ( 'NONE',  ( -2.750000000000000444, 7.339000000000001300, 3.161250000000001670 ) ) ;
#5237 = FACE_OUTER_BOUND ( 'NONE', #1775, .T. ) ;
#5238 = ORIENTED_EDGE ( 'NONE', *, *, #279, .F. ) ;
#5239 = PERSON_AND_ORGANIZATION ( #7862, #8117 ) ;
#5240 = ORIENTED_EDGE ( 'NONE', *, *, #7277, .T. ) ;
#5241 = DIRECTION ( 'NONE',  ( 0.000000000000000000, 0.000000000000000000, 1.000000000000000000 ) ) ;
#5242 = EDGE_CURVE ( 'NONE', #5914, #6240, #6948, .T. ) ;
#5243 = CARTESIAN_POINT ( 'NONE',  ( 0.000000000000000000, 1.750000000000000444, 0.000000000000000000 ) ) ;
#5244 = CARTESIAN_POINT ( 'NONE',  ( 4.462953385826773811, 4.225666661560477877, 8.231249998505111520 ) ) ;
#5245 = LINE ( 'NONE', #7798, #4879 ) ;
#5246 = ORIENTED_EDGE ( 'NONE', *, *, #2305, .T. ) ;
#5247 = EDGE_CURVE ( 'NONE', #41, #3907, #2040, .T. ) ;
#5248 = CARTESIAN_POINT ( 'NONE',  ( -4.936857409062767316E-17, 2.875000000000000444, 3.440250000000001140 ) ) ;
#5249 = DIRECTION ( 'NONE',  ( -1.000000000000000000, 0.000000000000000000, -2.606890220986081510E-17 ) ) ;
#5250 = ORIENTED_EDGE ( 'NONE', *, *, #6953, .T. ) ;
#5251 = COORDINATED_UNIVERSAL_TIME_OFFSET ( 0, 0, .AHEAD. ) ;
#5252 = CARTESIAN_POINT ( 'NONE',  ( 2.537500000000000533, 2.500000000000000444, -0.2625000000000008438 ) ) ;
#5253 = SECURITY_CLASSIFICATION_LEVEL ( 'unclassified' ) ;
#5254 = CARTESIAN_POINT ( 'NONE',  ( 0.7456179150311873505, 3.868434268270091625, 7.929405685993586417 ) ) ;
#5255 = CARTESIAN_POINT ( 'NONE',  ( -1.557862129405290341, 2.150738729984251307, -2.750000000000000444 ) ) ;
#5256 = CC_DESIGN_PERSON_AND_ORGANIZATION_ASSIGNMENT ( #2923, #8025, ( #1432 ) ) ;
#5257 = ORIENTED_EDGE ( 'NONE', *, *, #162, .T. ) ;
#5258 = CARTESIAN_POINT ( 'NONE',  ( 0.000000000000000000, 2.523992677165354248, 5.972081456692916568 ) ) ;
#5259 = VECTOR ( 'NONE', #8013, 39.37007874015748143 ) ;
#5260 = LOCAL_TIME ( 0, 37, 23.00000000000000000, #3108 ) ;
#5261 = EDGE_CURVE ( 'NONE', #4377, #1364, #7679, .T. ) ;
#5262 = CARTESIAN_POINT ( 'NONE',  ( -3.987046614173229475, 4.063153587259359156, 8.391936332830987055 ) ) ;
#5263 = ORIENTED_EDGE ( 'NONE', *, *, #3394, .T. ) ;
#5264 = CARTESIAN_POINT ( 'NONE',  ( 1.625000000000000222, 2.217843349262734076, -2.674602989435063805 ) ) ;
#5265 = VERTEX_POINT ( 'NONE', #5016 ) ;
#5266 = DIRECTION ( 'NONE',  ( 7.142086257945775577E-16, 1.000000000000000000, 0.000000000000000000 ) ) ;
#5267 = PERSON_AND_ORGANIZATION_ROLE ( 'design_supplier' ) ;
#5268 = ORIENTED_EDGE ( 'NONE', *, *, #1330, .T. ) ;
#5269 = VECTOR ( 'NONE', #3575, 39.37007874015748143 ) ;
#5270 = CARTESIAN_POINT ( 'NONE',  ( 2.740000000000001545, 7.969000000000000306, 3.828750000000002096 ) ) ;
#5271 = CIRCLE ( 'NONE', #2797, 0.3625000012227142521 ) ;
#5272 = EDGE_CURVE ( 'NONE', #1007, #1456, #2031, .T. ) ;
#5273 = CARTESIAN_POINT ( 'NONE',  ( -0.6588841106301542849, 2.814050781761043840, -5.108750000000002345 ) ) ;
#5274 = CARTESIAN_POINT ( 'NONE',  ( -3.987046614173228587, 4.146499994074616779, 8.231249998505111520 ) ) ;
#5275 = AXIS2_PLACEMENT_3D ( 'NONE', #2098, #6403, #4551 ) ;
#5276 = DIRECTION ( 'NONE',  ( -0.000000000000000000, 1.000000000000000000, 0.000000000000000000 ) ) ;
#5277 = VECTOR ( 'NONE', #5773, 39.37007874015748143 ) ;
#5278 = CARTESIAN_POINT ( 'NONE',  ( -1.312500000000000222, 8.589000000000002188, 3.161250000126027970 ) ) ;
#5279 = ORIENTED_EDGE ( 'NONE', *, *, #784, .T. ) ;
#5280 = CALENDAR_DATE ( 2026, 8, 10 ) ;
#5281 = ORIENTED_EDGE ( 'NONE', *, *, #5387, .T. ) ;
#5282 = CARTESIAN_POINT ( 'NONE',  ( -0.7077600209949284071, 3.701565529548706657, 8.040603848493713457 ) ) ;
#5283 = AXIS2_PLACEMENT_3D ( 'NONE', #3768, #4301, #1725 ) ;
#5284 = AXIS2_PLACEMENT_3D ( 'NONE', #2352, #3660, #3535 ) ;
#5285 = DIRECTION ( 'NONE',  ( -1.000000000000000000, 0.000000000000000000, 0.000000000000000000 ) ) ;
#5286 = EDGE_CURVE ( 'NONE', #6986, #7136, #7580, .T. ) ;
#5287 = LINE ( 'NONE', #4717, #4745 ) ;
#5288 = VECTOR ( 'NONE', #7217, 39.37007874015748143 ) ;
#5289 = CLOSED_SHELL ( 'NONE', ( #2875, #2231, #398, #4221, #993, #3548, #2286, #6668, #1084, #4121, #4382, #4321, #8115, #190, #7435, #2638, #3978, #4676, #6789, #2082, #1433, #2026, #4689, #6575, #366, #4675, #8062, #1232, #3171, #781, #42, #899, #1221, #7797, #5638, #1572, #6153, #3507, #2057, #2687, #4220, #5324, #5948, #5221, #118, #4998, #5434, #1285, #7002, #487, #1740, #3012, #4703, #1585, #2280, #8, #1040, #6440, #6404, #13, #7141, #3294, #6276, #36, #3682, #7767 ) ) ;
#5290 = CARTESIAN_POINT ( 'NONE',  ( 3.987953385826771058, 4.012112954393902697, 8.417726902280632473 ) ) ;
#5291 = ORIENTED_EDGE ( 'NONE', *, *, #1660, .F. ) ;
#5292 = VECTOR ( 'NONE', #5217, 39.37007874015748143 ) ;
#5293 = VECTOR ( 'NONE', #6510, 39.37007874015748143 ) ;
#5294 = DIRECTION ( 'NONE',  ( 0.000000000000000000, 0.000000000000000000, -1.000000000000000000 ) ) ;
#5295 = DIRECTION ( 'NONE',  ( 1.000000000000000000, 0.000000000000000000, 0.000000000000000000 ) ) ;
#5296 = COORDINATED_UNIVERSAL_TIME_OFFSET ( 0, 0, .AHEAD. ) ;
#5297 = DIRECTION ( 'NONE',  ( 1.000000000000000000, 0.000000000000000000, 0.000000000000000000 ) ) ;
#5298 = SECURITY_CLASSIFICATION_LEVEL ( 'unclassified' ) ;
#5299 = CARTESIAN_POINT ( 'NONE',  ( 0.7457411423250318583, 4.032391550759110821, 7.929090657501173034 ) ) ;
#5300 = CARTESIAN_POINT ( 'NONE',  ( 2.750000000000000888, 7.964000000000000412, 3.333750000000001990 ) ) ;
#5301 = EDGE_CURVE ( 'NONE', #1456, #7113, #2075, .T. ) ;
#5302 = EDGE_LOOP ( 'NONE', ( #4576, #2373, #6374, #6246, #6525, #5447, #1558, #1604, #7330, #1484, #3811, #1448 ) ) ;
#5303 = VECTOR ( 'NONE', #7399, 39.37007874015748854 ) ;
#5304 = CARTESIAN_POINT ( 'NONE',  ( -2.375000000000000888, 5.137500000000001066, 6.956249999999999822 ) ) ;
#5305 = VECTOR ( 'NONE', #746, 39.37007874015748143 ) ;
#5306 = DIRECTION ( 'NONE',  ( -0.000000000000000000, 0.000000000000000000, 1.000000000000000000 ) ) ;
#5307 = ORIENTED_EDGE ( 'NONE', *, *, #6299, .F. ) ;
#5308 = CARTESIAN_POINT ( 'NONE',  ( 1.500000000000000444, 5.113999999999999879, 2.750000000058594907 ) ) ;
#5309 = ORIENTED_EDGE ( 'NONE', *, *, #1479, .F. ) ;
#5310 = PRODUCT_DEFINITION ( 'UNKNOWN', '', #5941, #6037 ) ;
#5311 = CARTESIAN_POINT ( 'NONE',  ( 0.000000000000000000, 0.000000000000000000, -0.000000000000000000 ) ) ;
#5312 = DIRECTION ( 'NONE',  ( 0.000000000000000000, -0.000000000000000000, 1.000000000000000000 ) ) ;
#5313 = COORDINATED_UNIVERSAL_TIME_OFFSET ( 0, 0, .AHEAD. ) ;
#5314 = ORIENTED_EDGE ( 'NONE', *, *, #3888, .F. ) ;
#5315 = AXIS2_PLACEMENT_3D ( 'NONE', #684, #1181, #3760 ) ;
#5316 = CIRCLE ( 'NONE', #1014, 4.805751768934915624 ) ;
#5317 = DIRECTION ( 'NONE',  ( -1.000000000000000000, 0.000000000000000000, 0.000000000000000000 ) ) ;
#5318 = CARTESIAN_POINT ( 'NONE',  ( -0.8008852849046133038, 2.909290603415537024, -5.108749999999998792 ) ) ;
#5319 = CARTESIAN_POINT ( 'NONE',  ( -0.3549540556708988270, 2.363917302189245451, 3.041896893698089244 ) ) ;
#5320 = CARTESIAN_POINT ( 'NONE',  ( -2.875000000000000888, 0.000000000000000000, -2.612499998777286780 ) ) ;
#5321 = DIRECTION ( 'NONE',  ( -0.000000000000000000, -1.000000000000000000, -0.000000000000000000 ) ) ;
#5322 = PERSON_AND_ORGANIZATION ( #7862, #8117 ) ;
#5323 = ORIENTED_EDGE ( 'NONE', *, *, #5184, .F. ) ;
#5324 = ADVANCED_FACE ( 'NONE', ( #3935 ), #2693, .F. ) ;
#5325 = CARTESIAN_POINT ( 'NONE',  ( 0.000000000000000000, 3.950000000000001954, 3.956250000000000266 ) ) ;
#5326 = CARTESIAN_POINT ( 'NONE',  ( -2.750000000000000444, 8.719000000000001194, 3.823750000000002647 ) ) ;
#5327 = EDGE_CURVE ( 'NONE', #1089, #4344, #3986, .T. ) ;
#5328 = DIRECTION ( 'NONE',  ( 0.000000000000000000, 0.000000000000000000, -1.000000000000000000 ) ) ;
#5329 = CARTESIAN_POINT ( 'NONE',  ( 3.987953385826773278, 3.962486853702427592, 8.427751303491342938 ) ) ;
#5330 =( BOUNDED_CURVE ( )  B_SPLINE_CURVE ( 3, ( #3588, #2969, #5462, #4228 ),
 .UNSPECIFIED., .F., .T. ) 
 B_SPLINE_CURVE_WITH_KNOTS ( ( 4, 4 ),
 ( 6.938893903907228378E-18, 0.09552853962307136793 ),
 .UNSPECIFIED. ) 
 CURVE ( )  GEOMETRIC_REPRESENTATION_ITEM ( )  RATIONAL_B_SPLINE_CURVE ( ( 0.8289196715399411719, 0.6626358114187893555, 0.5593999943213423531, 0.5192122202476002757 ) ) 
 REPRESENTATION_ITEM ( '' )  );
#5331 = VERTEX_POINT ( 'NONE', #2812 ) ;
#5332 = LOCAL_TIME ( 0, 37, 23.00000000000000000, #6231 ) ;
#5333 = EDGE_CURVE ( 'NONE', #3004, #8024, #992, .T. ) ;
#5334 = CARTESIAN_POINT ( 'NONE',  ( -3.987046614173229475, 4.145406495827572257, 8.207305520648951358 ) ) ;
#5335 = CARTESIAN_POINT ( 'NONE',  ( 1.347488133582466441, 2.365290550890831067, -2.749999999536767437 ) ) ;
#5336 = LINE ( 'NONE', #7893, #3619 ) ;
#5337 = CARTESIAN_POINT ( 'NONE',  ( -3.796513189164427260, 1.365923996832131609E-16, -2.946478859991638277 ) ) ;
#5338 = EDGE_LOOP ( 'NONE', ( #5323, #3220 ) ) ;
#5339 = PERSON_AND_ORGANIZATION ( #7862, #8117 ) ;
#5340 = LINE ( 'NONE', #3387, #6877 ) ;
#5341 = CARTESIAN_POINT ( 'NONE',  ( 2.750000000000000444, 8.574153543316302972, 3.323749999966777668 ) ) ;
#5342 = ADVANCED_FACE ( 'NONE', ( #3898 ), #7760, .T. ) ;
#5343 = ORIENTED_EDGE ( 'NONE', *, *, #6835, .F. ) ;
#5344 = CARTESIAN_POINT ( 'NONE',  ( 2.537499998660271761, 3.550000000000001155, -0.3883559095726498156 ) ) ;
#5345 = LINE ( 'NONE', #6527, #5833 ) ;
#5346 = CARTESIAN_POINT ( 'NONE',  ( -2.750000000000000444, 8.729000000000002757, 3.813750000000002416 ) ) ;
#5347 = DIRECTION ( 'NONE',  ( 0.7071067811865667796, -0.7071067811865281438, -0.000000000000000000 ) ) ;
#5348 = ORIENTED_EDGE ( 'NONE', *, *, #7148, .F. ) ;
#5349 = DATE_AND_TIME ( #2862, #2406 ) ;
#5350 = CARTESIAN_POINT ( 'NONE',  ( 0.000000000000000000, 3.950000000000000178, 3.691250000234376660 ) ) ;
#5351 = PLANE ( 'NONE',  #5058 ) ;
#5352 = APPROVAL_ROLE ( '' ) ;
#5353 = ORIENTED_EDGE ( 'NONE', *, *, #2877, .T. ) ;
#5354 = PERSON ( 'NAUO-PER11', 'UNSPECIFIED', 'UNSPECIFIED', ('UNSPECIFIED'), ('UNSPECIFIED'), ('UNSPECIFIED') ) ;
#5355 = PERSON ( 'NAUO-PER4', 'UNSPECIFIED', 'UNSPECIFIED', ('UNSPECIFIED'), ('UNSPECIFIED'), ('UNSPECIFIED') ) ;
#5356 = CARTESIAN_POINT ( 'NONE',  ( 1.625000000000000222, 3.950000000000000178, -2.750000000000000444 ) ) ;
#5357 = CARTESIAN_POINT ( 'NONE',  ( 2.750000000000000444, 7.964000000000000412, 3.833750000000001545 ) ) ;
#5358 = LINE ( 'NONE', #7783, #448 ) ;
#5359 =( CONVERSION_BASED_UNIT ( 'INCH', #2343 ) LENGTH_UNIT ( ) NAMED_UNIT ( #2564 ) );
#5360 = DIRECTION ( 'NONE',  ( 1.000000000000000000, 0.000000000000000000, 0.000000000000000000 ) ) ;
#5361 = APPROVAL_ROLE ( '' ) ;
#5362 = VERTEX_POINT ( 'NONE', #183 ) ;
#5363 = DIRECTION ( 'NONE',  ( -0.7071067811865474617, -0.000000000000000000, 0.7071067811865474617 ) ) ;
#5364 = CC_DESIGN_PERSON_AND_ORGANIZATION_ASSIGNMENT ( #7520, #1263, ( #8109 ) ) ;
#5365 = DIRECTION ( 'NONE',  ( 0.000000000000000000, 1.000000000000000000, -0.000000000000000000 ) ) ;
#5366 = CARTESIAN_POINT ( 'NONE',  ( 0.000000000000000000, 2.389005866141733492, 4.968462007874016706 ) ) ;
#5367 = EDGE_CURVE ( 'NONE', #5813, #7789, #6511, .T. ) ;
#5368 = CARTESIAN_POINT ( 'NONE',  ( -2.750000000000000444, 7.964000000000000412, 3.691250000000001030 ) ) ;
#5369 = CARTESIAN_POINT ( 'NONE',  ( -0.6829499219002717059, 3.640031188008939989, 8.190215189619557634 ) ) ;
#5370 = ORIENTED_EDGE ( 'NONE', *, *, #1470, .T. ) ;
#5371 = EDGE_CURVE ( 'NONE', #3123, #402, #7161, .T. ) ;
#5372 = CARTESIAN_POINT ( 'NONE',  ( -3.987046614173227699, 3.925026340409374370, 8.034752674066879763 ) ) ;
#5373 = DIRECTION ( 'NONE',  ( 0.000000000000000000, 0.000000000000000000, 1.000000000000000000 ) ) ;
#5374 = DIRECTION ( 'NONE',  ( -7.142086257945775577E-16, -1.000000000000000000, 0.000000000000000000 ) ) ;
#5375 = CARTESIAN_POINT ( 'NONE',  ( 2.537500000000000533, 2.500000000000000444, 0.000000000000000000 ) ) ;
#5376 = CARTESIAN_POINT ( 'NONE',  ( -2.750000000000000444, 8.729000000000002757, 3.833750000000001545 ) ) ;
#5377 = EDGE_LOOP ( 'NONE', ( #7761, #7072, #7342, #502 ) ) ;
#5378 = PERSON_AND_ORGANIZATION ( #7862, #8117 ) ;
#5379 = CARTESIAN_POINT ( 'NONE',  ( 2.815000007187133058, 1.000000000000000222, -3.895000001893596853 ) ) ;
#5380 = CARTESIAN_POINT ( 'NONE',  ( 0.7253895767696344477, 4.141339130655848244, 7.983341084825775980 ) ) ;
#5381 = DIRECTION ( 'NONE',  ( 1.000000000000000000, 0.000000000000000000, -0.000000000000000000 ) ) ;
#5382 = ORIENTED_EDGE ( 'NONE', *, *, #3735, .T. ) ;
#5383 = CARTESIAN_POINT ( 'NONE',  ( 0.000000000000000000, 5.137500000000000178, 6.956250000000000711 ) ) ;
#5384 = ORIENTED_EDGE ( 'NONE', *, *, #476, .F. ) ;
#5385 = CARTESIAN_POINT ( 'NONE',  ( -3.987046614173229031, 4.225666661560476989, 7.679916707260901809 ) ) ;
#5386 = DIRECTION ( 'NONE',  ( -0.000000000000000000, -1.000000000000000000, -0.000000000000000000 ) ) ;
#5387 = EDGE_CURVE ( 'NONE', #1923, #2064, #5966, .T. ) ;
#5388 = EDGE_LOOP ( 'NONE', ( #2434, #762, #8157, #6630 ) ) ;
#5389 = CALENDAR_DATE ( 2026, 8, 10 ) ;
#5390 = CARTESIAN_POINT ( 'NONE',  ( -2.740000000000001545, 7.964000000000000412, 4.313750000000002416 ) ) ;
#5391 = ORIENTED_EDGE ( 'NONE', *, *, #4387, .F. ) ;
#5392 = CARTESIAN_POINT ( 'NONE',  ( -2.740000000000001545, 7.964000000000000412, 3.833750000000001545 ) ) ;
#5393 = DIRECTION ( 'NONE',  ( -0.000000000000000000, -0.000000000000000000, 1.000000000000000000 ) ) ;
#5394 = CIRCLE ( 'NONE', #1866, 2.841000000000000636 ) ;
#5395 = CC_DESIGN_APPROVAL ( #4164, ( #7249 ) ) ;
#5396 = DIRECTION ( 'NONE',  ( 0.000000000000000000, 1.000000000000000000, 0.000000000000000000 ) ) ;
#5397 = CARTESIAN_POINT ( 'NONE',  ( -0.5081896104144416615, 2.405274364305883150, 3.001302249876916406 ) ) ;
#5398 = FACE_BOUND ( 'NONE', #1060, .T. ) ;
#5399 = DIRECTION ( 'NONE',  ( -0.7071067811865474617, -0.000000000000000000, 0.7071067811865474617 ) ) ;
#5400 = COORDINATED_UNIVERSAL_TIME_OFFSET ( 0, 0, .AHEAD. ) ;
#5401 = ORIENTED_EDGE ( 'NONE', *, *, #3820, .F. ) ;
#5402 = VECTOR ( 'NONE', #4165, 39.37007874015748854 ) ;
#5403 = CARTESIAN_POINT ( 'NONE',  ( -3.762484563843162988, 1.281112611882646579, -7.524969127686321535 ) ) ;
#5404 = LOCAL_TIME ( 0, 37, 23.00000000000000000, #4632 ) ;
#5405 = ADVANCED_FACE ( 'NONE', ( #3423 ), #2848, .T. ) ;
#5406 = VECTOR ( 'NONE', #4266, 39.37007874015748143 ) ;
#5407 = DIRECTION ( 'NONE',  ( 0.000000000000000000, -1.000000000000000000, 0.000000000000000000 ) ) ;
#5408 = CARTESIAN_POINT ( 'NONE',  ( 2.749999999999998668, 8.589000000000000412, 5.236250000000000071 ) ) ;
#5409 = DIRECTION ( 'NONE',  ( 1.000000000000000000, 0.000000000000000000, 0.000000000000000000 ) ) ;
#5410 = ORIENTED_EDGE ( 'NONE', *, *, #6849, .F. ) ;
#5411 = CC_DESIGN_PERSON_AND_ORGANIZATION_ASSIGNMENT ( #4711, #3325, ( #1877 ) ) ;
#5412 = LINE ( 'NONE', #1046, #8080 ) ;
#5413 = VERTEX_POINT ( 'NONE', #4685 ) ;
#5414 = AXIS2_PLACEMENT_3D ( 'NONE', #3659, #1122, #6236 ) ;
#5415 = B_SPLINE_CURVE_WITH_KNOTS ( 'NONE', 3,
 ( #1770, #4260, #7229, #5999 ),
 .UNSPECIFIED., .F., .F.,
 ( 4, 4 ),
 ( 0.000000000000000000, 1.000000000000000000 ),
 .UNSPECIFIED. ) ;
#5416 = AXIS2_PLACEMENT_3D ( 'NONE', #5151, #3154, #2051 ) ;
#5417 = CARTESIAN_POINT ( 'NONE',  ( -3.987046614173229475, 4.017233591675442916, 8.046596944803717122 ) ) ;
#5418 = VECTOR ( 'NONE', #7243, 39.37007874015748143 ) ;
#5419 =( GEOMETRIC_REPRESENTATION_CONTEXT ( 3 ) GLOBAL_UNCERTAINTY_ASSIGNED_CONTEXT ( ( #955 ) ) GLOBAL_UNIT_ASSIGNED_CONTEXT ( ( #2427, #1765, #1688 ) ) REPRESENTATION_CONTEXT ( 'NONE', 'WORKASPACE' ) );
#5420 = CARTESIAN_POINT ( 'NONE',  ( -8.751021560936518753E-10, 1.365923996832131609E-16, 5.750408897959578548E-10 ) ) ;
#5421 = EDGE_LOOP ( 'NONE', ( #2790, #2012, #6415, #81, #4958 ) ) ;
#5422 = APPROVAL_DATE_TIME ( #3590, #1375 ) ;
#5423 = CARTESIAN_POINT ( 'NONE',  ( 2.745000000000000995, 8.719000000000002970, 3.828750000000002096 ) ) ;
#5424 = CARTESIAN_POINT ( 'NONE',  ( 0.000000000000000000, 3.950000000000000178, 6.956250000000000711 ) ) ;
#5425 = LOCAL_TIME ( 0, 37, 23.00000000000000000, #4031 ) ;
#5426 = EDGE_LOOP ( 'NONE', ( #5401, #429, #640, #900 ) ) ;
#5427 = EDGE_CURVE ( 'NONE', #5331, #1089, #3296, .T. ) ;
#5428 = CARTESIAN_POINT ( 'NONE',  ( -1.624999999999999778, 3.950000000000000178, -5.108750000000001457 ) ) ;
#5429 = VERTEX_POINT ( 'NONE', #1587 ) ;
#5430 = DIRECTION ( 'NONE',  ( -0.000000000000000000, -1.000000000000000000, 0.000000000000000000 ) ) ;
#5431 = ORIENTED_EDGE ( 'NONE', *, *, #78, .F. ) ;
#5432 = APPROVAL_ROLE ( '' ) ;
#5433 = EDGE_CURVE ( 'NONE', #8139, #1295, #6594, .T. ) ;
#5434 = ADVANCED_FACE ( 'NONE', ( #7894 ), #4725, .F. ) ;
#5435 = DIRECTION ( 'NONE',  ( 0.000000000000000000, -1.000000000000000000, 0.000000000000000000 ) ) ;
#5436 = APPROVAL_STATUS ( 'not_yet_approved' ) ;
#5437 = ORIENTED_EDGE ( 'NONE', *, *, #4497, .T. ) ;
#5438 = CARTESIAN_POINT ( 'NONE',  ( -3.791570908345035740, 1.365923996832131609E-16, 0.7997593681799632925 ) ) ;
#5439 = CARTESIAN_POINT ( 'NONE',  ( 0.1300012438279209703, 2.329874691800032149, 3.075403168634932349 ) ) ;
#5440 = CARTESIAN_POINT ( 'NONE',  ( -0.7491290119348464893, 3.991397162765705442, 7.920824285553324628 ) ) ;
#5441 = ADVANCED_BREP_SHAPE_REPRESENTATION ( '', ( #7251, #7272 ), #2811 ) ;
#5442 = CARTESIAN_POINT ( 'NONE',  ( 3.362500000000001155, 1.750000000000000222, 6.725000000000002309 ) ) ;
#5443 = AXIS2_PLACEMENT_3D ( 'NONE', #638, #5010, #1253 ) ;
#5444 = CIRCLE ( 'NONE', #3998, 3.343750000000001332 ) ;
#5445 = APPLICATION_PROTOCOL_DEFINITION ( 'international standard', 'config_control_design', 1994, #4403 ) ;
#5446 = VECTOR ( 'NONE', #3541, 39.37007874015748143 ) ;
#5447 = ORIENTED_EDGE ( 'NONE', *, *, #2634, .T. ) ;
#5448 = LINE ( 'NONE', #6035, #492 ) ;
#5449 = B_SPLINE_CURVE_WITH_KNOTS ( 'NONE', 3,
 ( #4280, #7474, #1250, #6783, #1824, #3667, #7551, #4316, #6165, #1291, #6820, #3743, #1203, #6203, #3702, #5589, #8151, #1900, #4396, #3781, #1132, #1944, #6286, #3633, #6129, #7032 ),
 .UNSPECIFIED., .F., .F.,
 ( 4, 2, 2, 2, 2, 2, 2, 2, 2, 2, 2, 2, 4 ),
 ( 2.795095972151323432E-13, 0.01867100407285308614, 0.02800650610913988509, 0.03734200814542668750, 0.04667751018171348298, 0.05134526119985691195, 0.05601301221800034785, 0.06068076323614376988, 0.06534851425428719884, 0.06768238976335887169, 0.07001626527243054454, 0.07235014078150221739, 0.07468401629057389024 ),
 .UNSPECIFIED. ) ;
#5450 = ADVANCED_FACE ( 'NONE', ( #5177 ), #7118, .F. ) ;
#5451 = AXIS2_PLACEMENT_3D ( 'NONE', #5392, #4078, #1722 ) ;
#5452 = DIRECTION ( 'NONE',  ( 0.000000000000000000, 0.000000000000000000, -1.000000000000000000 ) ) ;
#5453 = LINE ( 'NONE', #299, #5175 ) ;
#5454 = ORIENTED_EDGE ( 'NONE', *, *, #4109, .F. ) ;
#5455 = CARTESIAN_POINT ( 'NONE',  ( -3.296097360979716839, 1.749999999818133034, 0.5625000000000002220 ) ) ;
#5456 = VERTEX_POINT ( 'NONE', #2727 ) ;
#5457 = AXIS2_PLACEMENT_3D ( 'NONE', #5817, #5152, #859 ) ;
#5458 = ADVANCED_BREP_SHAPE_REPRESENTATION ( '', ( #1846, #7272 ), #1513 ) ;
#5459 = APPROVAL ( #4384, 'UNSPECIFIED' ) ;
#5460 = DIRECTION ( 'NONE',  ( -0.000000000000000000, 1.000000000000000000, 0.000000000000000000 ) ) ;
#5461 = CARTESIAN_POINT ( 'NONE',  ( -3.987046614173228143, 3.757075529380089485, 8.268572589389572514 ) ) ;
#5462 = CARTESIAN_POINT ( 'NONE',  ( -2.778020868884695460, 1.000000000000000000, 3.052064782510599095 ) ) ;
#5463 = CARTESIAN_POINT ( 'NONE',  ( -1.624999999336056877, 2.076218724820237060, -2.750000000000000444 ) ) ;
#5464 = ORIENTED_EDGE ( 'NONE', *, *, #1193, .F. ) ;
#5465 = DATE_AND_TIME ( #7245, #4357 ) ;
#5466 = DIRECTION ( 'NONE',  ( 0.7071067811865475727, -0.7071067811865475727, 0.000000000000000000 ) ) ;
#5467 = ORIENTED_EDGE ( 'NONE', *, *, #7681, .T. ) ;
#5468 = DIRECTION ( 'NONE',  ( 0.000000000000000000, 0.000000000000000000, -1.000000000000000000 ) ) ;
#5469 = CARTESIAN_POINT ( 'NONE',  ( -3.343750000000001776, 0.000000000000000000, -0.5624999982030005619 ) ) ;
#5470 = DIRECTION ( 'NONE',  ( 0.000000000000000000, 0.000000000000000000, -1.000000000000000000 ) ) ;
#5471 = ORIENTED_EDGE ( 'NONE', *, *, #4641, .F. ) ;
#5472 = PERSON_AND_ORGANIZATION_ROLE ( 'creator' ) ;
#5473 = DIRECTION ( 'NONE',  ( -0.000000000000000000, -1.000000000000000000, -0.000000000000000000 ) ) ;
#5474 = CARTESIAN_POINT ( 'NONE',  ( -0.7491290119348461563, 3.908602837234294913, 8.541675714446675727 ) ) ;
#5475 = CARTESIAN_POINT ( 'NONE',  ( -0.1707770274186259651, 5.254148146219773885, -5.108750000000001457 ) ) ;
#5476 = CALENDAR_DATE ( 2026, 8, 10 ) ;
#5477 = CARTESIAN_POINT ( 'NONE',  ( -1.187500000000000666, 7.339000000000003965, 4.267772478942485570 ) ) ;
#5478 = ADVANCED_FACE ( 'NONE', ( #797 ), #1506, .F. ) ;
#5479 = EDGE_CURVE ( 'NONE', #7981, #1117, #7689, .T. ) ;
#5480 = EDGE_CURVE ( 'NONE', #5222, #822, #2361, .T. ) ;
#5481 = DIRECTION ( 'NONE',  ( 0.000000000000000000, 0.000000000000000000, -1.000000000000000000 ) ) ;
#5482 = CARTESIAN_POINT ( 'NONE',  ( 2.187663376927555706E-18, 3.950000000000000178, 0.1249999999999997641 ) ) ;
#5483 = EDGE_LOOP ( 'NONE', ( #3843, #7609 ) ) ;
#5484 = FACE_OUTER_BOUND ( 'NONE', #7562, .T. ) ;
#5485 = DIRECTION ( 'NONE',  ( 1.000000000000000000, 0.000000000000000000, -0.000000000000000000 ) ) ;
#5486 = SHAPE_DEFINITION_REPRESENTATION ( #100, #6762 ) ;
#5487 = VERTEX_POINT ( 'NONE', #1707 ) ;
#5488 = CARTESIAN_POINT ( 'NONE',  ( 0.7499999999999993339, 3.950000000000000178, 7.231250000000000178 ) ) ;
#5489 = PRODUCT_DEFINITION_SHAPE ( 'NONE', 'NONE',  #7978 ) ;
#5490 = ORIENTED_EDGE ( 'NONE', *, *, #4842, .T. ) ;
#5491 = CARTESIAN_POINT ( 'NONE',  ( -2.740000000000000213, 8.729000000000002757, 3.813750000000002416 ) ) ;
#5492 = LINE ( 'NONE', #1158, #826 ) ;
#5493 = EDGE_CURVE ( 'NONE', #7297, #3620, #4892, .T. ) ;
#5494 = ORIENTED_EDGE ( 'NONE', *, *, #4168, .T. ) ;
#5495 = DIRECTION ( 'NONE',  ( -0.000000000000000000, 1.000000000000000000, 0.000000000000000000 ) ) ;
#5496 = EDGE_LOOP ( 'NONE', ( #1402, #5134, #1281, #2133 ) ) ;
#5497 = CC_DESIGN_APPROVAL ( #5566, ( #449 ) ) ;
#5498 = CARTESIAN_POINT ( 'NONE',  ( 3.987953385826772390, 4.146499994074615003, 8.231249998505111520 ) ) ;
#5499 = LINE ( 'NONE', #1202, #3061 ) ;
#5500 = CARTESIAN_POINT ( 'NONE',  ( 3.651126734928074491, 1.365923996832131609E-16, -1.298036420927624501 ) ) ;
#5501 = LINE ( 'NONE', #7511, #3737 ) ;
#5502 = ORIENTED_EDGE ( 'NONE', *, *, #3996, .T. ) ;
#5503 = COORDINATED_UNIVERSAL_TIME_OFFSET ( 0, 0, .AHEAD. ) ;
#5504 = PLANE ( 'NONE',  #6235 ) ;
#5505 = EDGE_CURVE ( 'NONE', #5594, #2439, #1367, .T. ) ;
#5506 = VERTEX_POINT ( 'NONE', #3508 ) ;
#5507 = EDGE_CURVE ( 'NONE', #987, #7723, #1623, .T. ) ;
#5508 = CARTESIAN_POINT ( 'NONE',  ( 2.875000000000000888, -3.820994292482255198E-18, -3.337500001222715174 ) ) ;
#5509 = FACE_OUTER_BOUND ( 'NONE', #7274, .T. ) ;
#5510 = ORIENTED_EDGE ( 'NONE', *, *, #1163, .T. ) ;
#5511 = PERSON_AND_ORGANIZATION ( #7862, #8117 ) ;
#5512 = CARTESIAN_POINT ( 'NONE',  ( 0.7335700393700786970, 2.500000000000000444, 2.909883779527559611 ) ) ;
#5513 = SECURITY_CLASSIFICATION_LEVEL ( 'unclassified' ) ;
#5514 = CC_DESIGN_DATE_AND_TIME_ASSIGNMENT ( #308, #475, ( #6195 ) ) ;
#5515 = CARTESIAN_POINT ( 'NONE',  ( 4.476342532109287120, 3.950000015938371689, 8.231249998505111520 ) ) ;
#5516 = EDGE_CURVE ( 'NONE', #6151, #3620, #4853, .T. ) ;
#5517 = PLANE ( 'NONE',  #3047 ) ;
#5518 = ORIENTED_EDGE ( 'NONE', *, *, #5507, .F. ) ;
#5519 = CARTESIAN_POINT ( 'NONE',  ( -0.7371834602650290114, 4.089377917019955788, 7.950806627216492117 ) ) ;
#5520 = FACE_OUTER_BOUND ( 'NONE', #5012, .T. ) ;
#5521 = CARTESIAN_POINT ( 'NONE',  ( 3.121988307086614345, 5.510994133858267752, 4.968462007874016706 ) ) ;
#5522 = APPROVAL_DATE_TIME ( #4303, #4313 ) ;
#5523 = ORIENTED_EDGE ( 'NONE', *, *, #3023, .F. ) ;
#5524 = ADVANCED_FACE ( 'NONE', ( #8064 ), #1787, .T. ) ;
#5525 = DIRECTION ( 'NONE',  ( 7.142086257945775577E-16, 1.000000000000000000, 0.000000000000000000 ) ) ;
#5526 = AXIS2_PLACEMENT_3D ( 'NONE', #6289, #4473, #3136 ) ;
#5527 = LOCAL_TIME ( 0, 37, 23.00000000000000000, #7311 ) ;
#5528 = ORIENTED_EDGE ( 'NONE', *, *, #3289, .T. ) ;
#5529 = CARTESIAN_POINT ( 'NONE',  ( -2.740000000000000213, 8.729000000000002757, 3.823750000000002647 ) ) ;
#5530 = AXIS2_PLACEMENT_3D ( 'NONE', #2393, #4807, #4217 ) ;
#5531 = VECTOR ( 'NONE', #305, 39.37007874015748143 ) ;
#5532 = CARTESIAN_POINT ( 'NONE',  ( -0.7499999999999993339, 3.950000000000000622, 8.543750000000002842 ) ) ;
#5533 = LOCAL_TIME ( 0, 37, 23.00000000000000000, #2850 ) ;
#5534 = EDGE_LOOP ( 'NONE', ( #325, #1472, #4014, #854 ) ) ;
#5535 = ORIENTED_EDGE ( 'NONE', *, *, #942, .F. ) ;
#5536 = VECTOR ( 'NONE', #3834, 39.37007874015748143 ) ;
#5537 = ADVANCED_FACE ( 'NONE', ( #6704 ), #6006, .T. ) ;
#5538 = ADVANCED_FACE ( 'NONE', ( #428 ), #7378, .T. ) ;
#5539 = CARTESIAN_POINT ( 'NONE',  ( 3.987953385826772390, 4.116323182045893425, 8.126559114046001397 ) ) ;
#5540 = CARTESIAN_POINT ( 'NONE',  ( -3.987046614173228587, 3.757384381775306093, 8.270135292618874701 ) ) ;
#5541 = DIRECTION ( 'NONE',  ( 0.000000000000000000, 0.000000000000000000, 1.000000000000000000 ) ) ;
#5542 = CARTESIAN_POINT ( 'NONE',  ( 3.484361157547035681, 0.9999999999999639178, -1.767115912903641339 ) ) ;
#5543 = EDGE_LOOP ( 'NONE', ( #170, #6432, #2561, #4819, #6022, #1013 ) ) ;
#5544 = DATE_AND_TIME ( #5053, #561 ) ;
#5545 = AXIS2_PLACEMENT_3D ( 'NONE', #4657, #2124, #855 ) ;
#5546 = CARTESIAN_POINT ( 'NONE',  ( -3.362499999999999822, 1.750000000000000222, 6.725000000000002309 ) ) ;
#5547 = APPLICATION_CONTEXT ( 'configuration controlled 3d designs of mechanical parts and assemblies' ) ;
#5548 = SHAPE_REPRESENTATION ( 'bench vise6-', ( #7272 ), #720 ) ;
#5549 = EDGE_CURVE ( 'NONE', #2981, #6439, #7931, .T. ) ;
#5550 = EDGE_LOOP ( 'NONE', ( #2085, #5343, #904, #4059, #4876, #3128, #2636, #2694, #5118, #90, #4643, #5211 ) ) ;
#5551 = CIRCLE ( 'NONE', #7422, 2.845000000000001528 ) ;
#5552 = CARTESIAN_POINT ( 'NONE',  ( -2.815000008655331509, 1.000000000000000444, -3.895000002097408043 ) ) ;
#5553 = PLANE ( 'NONE',  #2810 ) ;
#5554 = FACE_OUTER_BOUND ( 'NONE', #6665, .T. ) ;
#5555 = ORIENTED_EDGE ( 'NONE', *, *, #4439, .T. ) ;
#5556 = APPROVAL_STATUS ( 'not_yet_approved' ) ;
#5557 = CARTESIAN_POINT ( 'NONE',  ( -8.751021560936518753E-10, 1.000000000000000222, 5.750408897959578548E-10 ) ) ;
#5558 = EDGE_CURVE ( 'NONE', #3668, #4859, #6088, .T. ) ;
#5559 = VECTOR ( 'NONE', #3602, 39.37007874015748143 ) ;
#5560 = DIRECTION ( 'NONE',  ( 1.000000000000000000, 0.000000000000000000, 0.000000000000000000 ) ) ;
#5561 = AXIS2_PLACEMENT_3D ( 'NONE', #2050, #4659, #7175 ) ;
#5562 = PRODUCT_DEFINITION_SHAPE ( 'NONE', 'NONE',  #6424 ) ;
#5563 = AXIS2_PLACEMENT_3D ( 'NONE', #7391, #6175, #556 ) ;
#5564 = CARTESIAN_POINT ( 'NONE',  ( 0.000000000000000000, 2.325000000000000622, -3.080208333333334103 ) ) ;
#5565 = DIRECTION ( 'NONE',  ( 0.000000000000000000, 0.000000000000000000, -1.000000000000000000 ) ) ;
#5566 = APPROVAL ( #4595, 'UNSPECIFIED' ) ;
#5567 = CARTESIAN_POINT ( 'NONE',  ( 0.000000000000000000, 0.000000000000000000, -0.000000000000000000 ) ) ;
#5568 = ORIENTED_EDGE ( 'NONE', *, *, #6187, .T. ) ;
#5569 = CARTESIAN_POINT ( 'NONE',  ( -0.6955978521287335958, 4.230565908133124609, 8.370402240390433235 ) ) ;
#5570 = CARTESIAN_POINT ( 'NONE',  ( 2.750000000000000444, 7.531471846334603981, 3.702890677416158294 ) ) ;
#5571 = DIRECTION ( 'NONE',  ( -0.000000000000000000, -0.000000000000000000, 1.000000000000000000 ) ) ;
#5572 = CARTESIAN_POINT ( 'NONE',  ( 0.000000000000000000, 5.541000000000003034, 3.956250000000000266 ) ) ;
#5573 = COORDINATED_UNIVERSAL_TIME_OFFSET ( 0, 0, .AHEAD. ) ;
#5574 = ORIENTED_EDGE ( 'NONE', *, *, #7159, .T. ) ;
#5575 = CARTESIAN_POINT ( 'NONE',  ( -3.562500000000000444, -3.820994442221351629E-18, 2.612499999999998934 ) ) ;
#5576 = EDGE_CURVE ( 'NONE', #266, #7256, #6782, .T. ) ;
#5577 = VERTEX_POINT ( 'NONE', #7295 ) ;
#5578 = CARTESIAN_POINT ( 'NONE',  ( 1.500000000000000444, 5.339000000000000412, -2.750000000000000444 ) ) ;
#5579 = AXIS2_PLACEMENT_3D ( 'NONE', #1715, #484, #2372 ) ;
#5580 = CARTESIAN_POINT ( 'NONE',  ( 0.000000000000000000, 3.001975734461090560E-16, 0.000000000000000000 ) ) ;
#5581 = ORIENTED_EDGE ( 'NONE', *, *, #1200, .T. ) ;
#5582 = ADVANCED_FACE ( 'NONE', ( #4144 ), #6164, .T. ) ;
#5583 = ORIENTED_EDGE ( 'NONE', *, *, #5584, .F. ) ;
#5584 = EDGE_CURVE ( 'NONE', #6974, #6859, #4626, .T. ) ;
#5585 = VECTOR ( 'NONE', #7605, 39.37007874015748143 ) ;
#5586 = EDGE_CURVE ( 'NONE', #6055, #6810, #1741, .T. ) ;
#5587 = CARTESIAN_POINT ( 'NONE',  ( -0.6797036848942895615, 2.472748453411862446, -2.935395484029501123 ) ) ;
#5588 = DIRECTION ( 'NONE',  ( 0.000000000000000000, -1.000000000000000000, 0.000000000000000000 ) ) ;
#5589 = CARTESIAN_POINT ( 'NONE',  ( 1.187500000000000444, 4.474559027700158786, 6.463727320098461959 ) ) ;
#5590 = ORIENTED_EDGE ( 'NONE', *, *, #6984, .T. ) ;
#5591 = CIRCLE ( 'NONE', #7462, 2.841000000000000636 ) ;
#5592 = PERSON_AND_ORGANIZATION ( #7862, #8117 ) ;
#5593 = CARTESIAN_POINT ( 'NONE',  ( -1.312500000000000444, 5.969165905511811587, 3.161250000000001670 ) ) ;
#5594 = VERTEX_POINT ( 'NONE', #2450 ) ;
#5595 = CARTESIAN_POINT ( 'NONE',  ( 2.750000000000000888, 8.729000000000002757, 3.823750000000002647 ) ) ;
#5596 = CARTESIAN_POINT ( 'NONE',  ( 0.000000000000000000, 5.238734212598425088, 3.956250000000001155 ) ) ;
#5597 = CARTESIAN_POINT ( 'NONE',  ( 2.750000000000000444, 8.574153543316302972, 3.323749999966777668 ) ) ;
#5598 =( REPRESENTATION_RELATIONSHIP ('NONE','NONE', #3256, #3570 ) REPRESENTATION_RELATIONSHIP_WITH_TRANSFORMATION ( #648 )SHAPE_REPRESENTATION_RELATIONSHIP( ) );
#5599 = ORIENTED_EDGE ( 'NONE', *, *, #6152, .T. ) ;
#5600 = COORDINATED_UNIVERSAL_TIME_OFFSET ( 0, 0, .AHEAD. ) ;
#5601 = EDGE_CURVE ( 'NONE', #4502, #7088, #5330, .T. ) ;
#5602 = SECURITY_CLASSIFICATION_LEVEL ( 'unclassified' ) ;
#5603 = CARTESIAN_POINT ( 'NONE',  ( 0.7499999999999993339, 3.950000000000000178, 7.231250000000000178 ) ) ;
#5604 = CARTESIAN_POINT ( 'NONE',  ( 2.815000007187132613, 1.365923996832131609E-16, -3.895000001893597297 ) ) ;
#5605 = LOCAL_TIME ( 0, 37, 23.00000000000000000, #6269 ) ;
#5606 = CARTESIAN_POINT ( 'NONE',  ( -3.296097360979716839, 1.749999999818133034, 0.5625000000000002220 ) ) ;
#5607 = CARTESIAN_POINT ( 'NONE',  ( 2.778020867214854750, 1.000000000000000000, 3.052064783514492063 ) ) ;
#5608 = ORIENTED_EDGE ( 'NONE', *, *, #4834, .F. ) ;
#5609 = CARTESIAN_POINT ( 'NONE',  ( -4.462046614173230452, 3.674333370316265057, 8.231249998505111520 ) ) ;
#5610 = CARTESIAN_POINT ( 'NONE',  ( -2.740000000000000213, 8.729000000000002757, 3.813750000000002416 ) ) ;
#5611 = FACE_OUTER_BOUND ( 'NONE', #70, .T. ) ;
#5612 = DATE_AND_TIME ( #7012, #5332 ) ;
#5613 = ORIENTED_EDGE ( 'NONE', *, *, #1049, .F. ) ;
#5614 = DIRECTION ( 'NONE',  ( 1.000000000000000000, 0.000000000000000000, 0.000000000000000000 ) ) ;
#5615 = CC_DESIGN_PERSON_AND_ORGANIZATION_ASSIGNMENT ( #1551, #5922, ( #600 ) ) ;
#5616 = ADVANCED_FACE ( 'NONE', ( #7337 ), #6747, .T. ) ;
#5617 = CARTESIAN_POINT ( 'NONE',  ( -3.179822820373745085, 2.000074507330735329, -0.5624999982030005619 ) ) ;
#5618 = DIRECTION ( 'NONE',  ( 1.000000000000000000, 0.000000000000000000, 0.000000000000000000 ) ) ;
#5619 = ORIENTED_EDGE ( 'NONE', *, *, #4152, .T. ) ;
#5620 = EDGE_LOOP ( 'NONE', ( #5935, #3170, #715, #7900 ) ) ;
#5621 = APPROVAL ( #1213, 'UNSPECIFIED' ) ;
#5622 = LINE ( 'NONE', #2998, #6728 ) ;
#5623 = EDGE_CURVE ( 'NONE', #1500, #1742, #2146, .T. ) ;
#5624 = CARTESIAN_POINT ( 'NONE',  ( 0.9878476365635346923, 3.081585747833998745, -5.108750000000003233 ) ) ;
#5625 = ORIENTED_EDGE ( 'NONE', *, *, #187, .T. ) ;
#5626 = CALENDAR_DATE ( 2026, 8, 10 ) ;
#5627 = CARTESIAN_POINT ( 'NONE',  ( 3.987953385826772390, 3.753500037802128375, 8.231249998505111520 ) ) ;
#5628 = ORIENTED_EDGE ( 'NONE', *, *, #926, .F. ) ;
#5629 = EDGE_CURVE ( 'NONE', #3411, #5792, #4465, .T. ) ;
#5630 = CARTESIAN_POINT ( 'NONE',  ( 0.000000000000000000, 5.536672282146935409, 4.083473622047245399 ) ) ;
#5631 = CARTESIAN_POINT ( 'NONE',  ( 1.624999999999999778, 3.950000000000000178, -5.108750000000001457 ) ) ;
#5632 = CARTESIAN_POINT ( 'NONE',  ( 2.724999998660272205, 3.550000000000001155, 2.790532913385826763 ) ) ;
#5633 = ORIENTED_EDGE ( 'NONE', *, *, #3419, .T. ) ;
#5634 = PERSON_AND_ORGANIZATION_ROLE ( 'classification_officer' ) ;
#5635 = DIRECTION ( 'NONE',  ( -0.000000000000000000, -1.000000000000000000, -0.000000000000000000 ) ) ;
#5636 = ITEM_DEFINED_TRANSFORMATION ( 'NONE', 'NONE', #858,  #7272 ) ;
#5637 = CARTESIAN_POINT ( 'NONE',  ( -1.274606804509407887, 2.434036455836466217, 2.750000000000000444 ) ) ;
#5638 = ADVANCED_FACE ( 'NONE', ( #209 ), #2750, .F. ) ;
#5639 = CARTESIAN_POINT ( 'NONE',  ( -3.987046614173228143, 3.801472271119497037, 8.101886876862232967 ) ) ;
#5640 = DIRECTION ( 'NONE',  ( -0.000000000000000000, 1.000000000000000000, -0.000000000000000000 ) ) ;
#5641 = DIRECTION ( 'NONE',  ( 0.000000000000000000, 0.000000000000000000, 1.000000000000000000 ) ) ;
#5642 = EDGE_LOOP ( 'NONE', ( #6717, #6138, #5830, #5978, #2047, #1734 ) ) ;
#5643 = DIRECTION ( 'NONE',  ( -0.000000000000000000, 1.000000000000000000, -0.000000000000000000 ) ) ;
#5644 = CARTESIAN_POINT ( 'NONE',  ( 2.750000000000000444, 7.339000000000003077, 4.175863149606300340 ) ) ;
#5645 = APPROVAL_STATUS ( 'not_yet_approved' ) ;
#5646 =( BOUNDED_CURVE ( )  B_SPLINE_CURVE ( 3, ( #6274, #7098, #2670, #1318 ),
 .UNSPECIFIED., .F., .T. ) 
 B_SPLINE_CURVE_WITH_KNOTS ( ( 4, 4 ),
 ( 0.000000000000000000, 1.000000000000000000 ),
 .UNSPECIFIED. ) 
 CURVE ( )  GEOMETRIC_REPRESENTATION_ITEM ( )  RATIONAL_B_SPLINE_CURVE ( ( 1.000000000000000000, 0.3333333333333332038, 0.3333333333333332038, 1.000000000000000000 ) ) 
 REPRESENTATION_ITEM ( '' )  );
#5647 = VERTEX_POINT ( 'NONE', #2674 ) ;
#5648 = DIRECTION ( 'NONE',  ( 1.000000000000000000, 0.000000000000000000, 0.000000000000000000 ) ) ;
#5649 = CARTESIAN_POINT ( 'NONE',  ( -4.462046614173229564, 4.146499994074616779, 8.231249998505111520 ) ) ;
#5650 = DIRECTION ( 'NONE',  ( 0.000000000000000000, 0.000000000000000000, 1.000000000000000000 ) ) ;
#5651 = APPLICATION_CONTEXT ( 'configuration controlled 3d designs of mechanical parts and assemblies' ) ;
#5652 = VECTOR ( 'NONE', #7889, 39.37007874015748143 ) ;
#5653 = ORIENTED_EDGE ( 'NONE', *, *, #187, .F. ) ;
#5654 = ORIENTED_EDGE ( 'NONE', *, *, #4388, .T. ) ;
#5655 = AXIS2_PLACEMENT_3D ( 'NONE', #7237, #794, #3292 ) ;
#5656 = CIRCLE ( 'NONE', #7664, 5.349138356872925826 ) ;
#5657 = APPROVAL_PERSON_ORGANIZATION ( #844, #4164, #7638 ) ;
#5658 = CARTESIAN_POINT ( 'NONE',  ( -0.6239339750438661625, 2.448288917813445487, -2.959250064740976960 ) ) ;
#5659 = CC_DESIGN_PERSON_AND_ORGANIZATION_ASSIGNMENT ( #5322, #2222, ( #1877 ) ) ;
#5660 = CARTESIAN_POINT ( 'NONE',  ( 1.301660623806975448, 4.119709289672806030, -5.108750000000004121 ) ) ;
#5661 = DIRECTION ( 'NONE',  ( 0.7071067811865475727, 0.000000000000000000, -0.7071067811865475727 ) ) ;
#5662 = ORIENTED_EDGE ( 'NONE', *, *, #4625, .F. ) ;
#5663 = DATE_AND_TIME ( #5626, #3048 ) ;
#5664 = ORIENTED_EDGE ( 'NONE', *, *, #4040, .F. ) ;
#5665 = CARTESIAN_POINT ( 'NONE',  ( -2.750000000000000444, 8.574153543306394454, 3.323750000003751648 ) ) ;
#5666 = CARTESIAN_POINT ( 'NONE',  ( 0.000000000000000000, 2.500000000000000000, 0.000000000000000000 ) ) ;
#5667 = AXIS2_PLACEMENT_3D ( 'NONE', #5954, #2226, #7887 ) ;
#5668 = ORIENTED_EDGE ( 'NONE', *, *, #4634, .F. ) ;
#5669 = AXIS2_PLACEMENT_3D ( 'NONE', #5243, #6545, #1043 ) ;
#5670 = VECTOR ( 'NONE', #6670, 39.37007874015748143 ) ;
#5671 = VECTOR ( 'NONE', #6536, 39.37007874015748143 ) ;
#5672 = ADVANCED_FACE ( 'NONE', ( #6973 ), #7062, .F. ) ;
#5673 = FACE_OUTER_BOUND ( 'NONE', #7649, .T. ) ;
#5674 = CARTESIAN_POINT ( 'NONE',  ( 0.000000000000000000, 5.025000000000000355, 3.440250000000001140 ) ) ;
#5675 = DIRECTION ( 'NONE',  ( 0.000000000000000000, 1.000000000000000000, -0.000000000000000000 ) ) ;
#5676 = ORIENTED_EDGE ( 'NONE', *, *, #2551, .F. ) ;
#5677 = DATE_AND_TIME ( #3178, #3441 ) ;
#5678 = DIRECTION ( 'NONE',  ( 1.000000000000000000, 0.000000000000000000, 0.000000000000000000 ) ) ;
#5679 = COORDINATED_UNIVERSAL_TIME_OFFSET ( 0, 0, .AHEAD. ) ;
#5680 = CARTESIAN_POINT ( 'NONE',  ( 3.296097361251832503, 1.749999999892448477, 0.5624999982029994516 ) ) ;
#5681 = DIRECTION ( 'NONE',  ( 0.000000000000000000, 0.000000000000000000, -1.000000000000000000 ) ) ;
#5682 = VECTOR ( 'NONE', #6255, 39.37007874015748854 ) ;
#5683 = EDGE_CURVE ( 'NONE', #47, #6151, #786, .T. ) ;
#5684 = CARTESIAN_POINT ( 'NONE',  ( -3.987046614173229475, 3.866991449158490912, 8.053088436266007122 ) ) ;
#5685 = CARTESIAN_POINT ( 'NONE',  ( 1.124999999999999556, 3.950000000000000178, 7.131250000000001421 ) ) ;
#5686 = EDGE_CURVE ( 'NONE', #938, #2452, #6202, .T. ) ;
#5687 = DIRECTION ( 'NONE',  ( 0.000000000000000000, 0.000000000000000000, 1.000000000000000000 ) ) ;
#5688 = VERTEX_POINT ( 'NONE', #1445 ) ;
#5689 = CARTESIAN_POINT ( 'NONE',  ( -2.740000000000000657, 7.964000000000000412, 3.823750000000002647 ) ) ;
#5690 = CLOSED_SHELL ( 'NONE', ( #5538, #7489, #8095, #2018 ) ) ;
#5691 = DIRECTION ( 'NONE',  ( -0.000000000000000000, -1.000000000000000000, -0.000000000000000000 ) ) ;
#5692 = B_SPLINE_CURVE_WITH_KNOTS ( 'NONE', 3,
 ( #1466, #2081, #7765, #312, #7641, #6472 ),
 .UNSPECIFIED., .F., .F.,
 ( 4, 2, 4 ),
 ( 0.000000000000000000, 0.5000000000000000000, 1.000000000000000000 ),
 .UNSPECIFIED. ) ;
#5693 = CC_DESIGN_DATE_AND_TIME_ASSIGNMENT ( #6647, #6021, ( #267 ) ) ;
#5694 = CALENDAR_DATE ( 2026, 8, 10 ) ;
#5695 = ORIENTED_EDGE ( 'NONE', *, *, #8098, .F. ) ;
#5696 = CARTESIAN_POINT ( 'NONE',  ( -4.470366334113919926, 1.365923996832131609E-16, 2.937534001674282358 ) ) ;
#5697 = EDGE_CURVE ( 'NONE', #5031, #4344, #5122, .T. ) ;
#5698 = LOCAL_TIME ( 0, 37, 23.00000000000000000, #4827 ) ;
#5699 = DIMENSIONAL_EXPONENTS ( 1.000000000000000000, 0.000000000000000000, 0.000000000000000000, 0.000000000000000000, 0.000000000000000000, 0.000000000000000000, 0.000000000000000000 ) ;
#5700 = LINE ( 'NONE', #5744, #579 ) ;
#5701 = CARTESIAN_POINT ( 'NONE',  ( -3.796513189164425928, 1.365923996832131609E-16, -2.946478859991638277 ) ) ;
#5702 = DIRECTION ( 'NONE',  ( 0.000000000000000000, 0.000000000000000000, 1.000000000000000000 ) ) ;
#5703 = AXIS2_PLACEMENT_3D ( 'NONE', #5852, #2814, #5297 ) ;
#5704 = CIRCLE ( 'NONE', #2704, 1.249999999999999556 ) ;
#5705 = ORIENTED_EDGE ( 'NONE', *, *, #2205, .F. ) ;
#5706 = ORIENTED_EDGE ( 'NONE', *, *, #7047, .T. ) ;
#5707 = VECTOR ( 'NONE', #4296, 39.37007874015748854 ) ;
#5708 = EDGE_CURVE ( 'NONE', #1477, #4859, #2635, .T. ) ;
#5709 = DIRECTION ( 'NONE',  ( 0.000000000000000000, 0.000000000000000000, -1.000000000000000000 ) ) ;
#5710 = CARTESIAN_POINT ( 'NONE',  ( 0.7455319525492740684, 2.869584312975302254, -5.108750000000003233 ) ) ;
#5711 = LINE ( 'NONE', #6502, #4389 ) ;
#5712 = VERTEX_POINT ( 'NONE', #2594 ) ;
#5713 = CARTESIAN_POINT ( 'NONE',  ( 3.687499987877263408, 1.365923996832131609E-16, 3.874999999790588401 ) ) ;
#5714 = VECTOR ( 'NONE', #3101, 39.37007874015748143 ) ;
#5715 = CIRCLE ( 'NONE', #6523, 0.1875000000000006661 ) ;
#5716 = ORIENTED_EDGE ( 'NONE', *, *, #3820, .T. ) ;
#5717 = CC_DESIGN_PERSON_AND_ORGANIZATION_ASSIGNMENT ( #7057, #1441, ( #4146 ) ) ;
#5718 = VECTOR ( 'NONE', #6955, 39.37007874015748143 ) ;
#5719 = CYLINDRICAL_SURFACE ( 'NONE', #7456, 1.624999999999999778 ) ;
#5720 = VECTOR ( 'NONE', #1680, 39.37007874015748143 ) ;
#5721 = FACE_BOUND ( 'NONE', #4712, .T. ) ;
#5722 = CARTESIAN_POINT ( 'NONE',  ( 2.150000000000000799, 2.875000000000001332, 3.742515787401574645 ) ) ;
#5723 = ORIENTED_EDGE ( 'NONE', *, *, #1977, .T. ) ;
#5724 = PERSON_AND_ORGANIZATION_ROLE ( 'design_supplier' ) ;
#5725 = CARTESIAN_POINT ( 'NONE',  ( 4.462953385826772923, 3.753500037802130596, 8.624249954777599925 ) ) ;
#5726 = COORDINATED_UNIVERSAL_TIME_OFFSET ( 0, 0, .AHEAD. ) ;
#5727 = CARTESIAN_POINT ( 'NONE',  ( 2.750000000000000000, 7.521783347043601964, 3.691250000474207038 ) ) ;
#5728 = CARTESIAN_POINT ( 'NONE',  ( -0.8969581913071023038, 4.909142736075838620, -5.108749999999997904 ) ) ;
#5729 = CC_DESIGN_PERSON_AND_ORGANIZATION_ASSIGNMENT ( #1637, #2938, ( #516 ) ) ;
#5730 = ORIENTED_EDGE ( 'NONE', *, *, #3289, .F. ) ;
#5731 = CARTESIAN_POINT ( 'NONE',  ( -2.750000000000000444, 7.964000000000000412, 3.691250000000001030 ) ) ;
#5732 = DIRECTION ( 'NONE',  ( -1.000000000000000000, 0.000000000000000000, 0.000000000000000000 ) ) ;
#5733 = VERTEX_POINT ( 'NONE', #3324 ) ;
#5734 = CARTESIAN_POINT ( 'NONE',  ( -2.750000000000000444, 8.589000000000000412, 4.486250000000000959 ) ) ;
#5735 = EDGE_CURVE ( 'NONE', #5265, #2302, #7747, .T. ) ;
#5736 = DIRECTION ( 'NONE',  ( -0.7071067811865474617, 0.7071067811865474617, -0.000000000000000000 ) ) ;
#5737 = ADVANCED_FACE ( 'N', ( #3283 ), #5781, .F. ) ;
#5738 = CARTESIAN_POINT ( 'NONE',  ( -0.7455319445466856987, 5.030415712794154892, -5.108750000000001457 ) ) ;
#5739 = APPROVAL_STATUS ( 'not_yet_approved' ) ;
#5740 = APPROVAL_PERSON_ORGANIZATION ( #6150, #6638, #1074 ) ;
#5741 = ORIENTED_EDGE ( 'NONE', *, *, #6808, .F. ) ;
#5742 = FACE_OUTER_BOUND ( 'NONE', #3885, .T. ) ;
#5743 = ADVANCED_FACE ( 'NONE', ( #6363 ), #5747, .T. ) ;
#5744 = CARTESIAN_POINT ( 'NONE',  ( -2.740000000000001545, 7.964000000000000412, 3.823750000000002647 ) ) ;
#5745 = PRODUCT ( 'bench vise5-', 'bench vise5-', '', ( #1171 ) ) ;
#5746 = CARTESIAN_POINT ( 'NONE',  ( -1.187500000000000000, 5.969165905511811587, 4.238473622047244760 ) ) ;
#5747 = PLANE ( 'NONE',  #7268 ) ;
#5748 = VERTEX_POINT ( 'NONE', #1483 ) ;
#5749 = ORIENTED_EDGE ( 'NONE', *, *, #776, .F. ) ;
#5750 = CARTESIAN_POINT ( 'NONE',  ( 3.987953385826772390, 3.753500037802128375, 8.231249998505111520 ) ) ;
#5751 = EDGE_CURVE ( 'NONE', #2544, #2688, #3460, .T. ) ;
#5752 = EDGE_CURVE ( 'NONE', #7868, #540, #4593, .T. ) ;
#5753 = CARTESIAN_POINT ( 'NONE',  ( 0.2166614821407901181, 5.245203122673235185, -5.108749999999999680 ) ) ;
#5754 =( BOUNDED_SURFACE ( )  B_SPLINE_SURFACE ( 3, 3, ( 
 ( #5383, #5304, #2165, #1673 ),
 ( #2857, #5929, #4070, #5258 ),
 ( #3395, #2241, #5892, #4732 ),
 ( #316, #2819, #7253, #7990 ) ),
 .UNSPECIFIED., .F., .F., .F. ) 
 B_SPLINE_SURFACE_WITH_KNOTS ( ( 4, 4 ),
 ( 4, 4 ),
 ( 0.000000000000000000, 1.000000000000000000 ),
 ( 0.000000000000000000, 1.000000000000000000 ),
 .UNSPECIFIED. ) 
 GEOMETRIC_REPRESENTATION_ITEM ( )  RATIONAL_B_SPLINE_SURFACE ( (
 ( 1.000000000000000000, 0.3333333333333330373, 0.3333333333333330373, 1.000000000000000000),
 ( 0.9963935896217739341, 0.3321311965405909783, 0.3321311965405909783, 0.9963935896217739341),
 ( 0.9963935896217739341, 0.3321311965405909783, 0.3321311965405909783, 0.9963935896217739341),
 ( 1.000000000000000000, 0.3333333333333330373, 0.3333333333333330373, 1.000000000000000000) ) ) 
 REPRESENTATION_ITEM ( '' )  SURFACE ( )  );
#5755 = DIRECTION ( 'NONE',  ( 1.000000000000000000, 0.000000000000000000, 0.000000000000000000 ) ) ;
#5756 = ORIENTED_EDGE ( 'NONE', *, *, #5549, .T. ) ;
#5757 = CARTESIAN_POINT ( 'NONE',  ( 3.987953385826773278, 3.839697420785548321, 8.393904357314971421 ) ) ;
#5758 = EDGE_LOOP ( 'NONE', ( #4633, #528, #5110, #550 ) ) ;
#5759 = CARTESIAN_POINT ( 'NONE',  ( 3.343750000000002220, 2.499999999622846136, 0.5624999994009998172 ) ) ;
#5760 = CARTESIAN_POINT ( 'NONE',  ( 1.187500000000000444, 8.523567380006621619, 4.820336057633928917 ) ) ;
#5761 = ORIENTED_EDGE ( 'NONE', *, *, #1489, .T. ) ;
#5762 = PERSON_AND_ORGANIZATION ( #7862, #8117 ) ;
#5763 = DIRECTION ( 'NONE',  ( 0.08785522444269551479, -0.000000000000000000, 0.9961332539063855185 ) ) ;
#5764 = FACE_OUTER_BOUND ( 'NONE', #3836, .T. ) ;
#5765 = DIRECTION ( 'NONE',  ( 0.000000000000000000, -1.000000000000000000, 0.000000000000000000 ) ) ;
#5766 = LINE ( 'NONE', #6917, #1355 ) ;
#5767 = EDGE_CURVE ( 'NONE', #4304, #5914, #585, .T. ) ;
#5768 = ORIENTED_EDGE ( 'NONE', *, *, #1683, .T. ) ;
#5769 = LINE ( 'NONE', #6347, #6617 ) ;
#5770 = LINE ( 'NONE', #689, #742 ) ;
#5771 = CARTESIAN_POINT ( 'NONE',  ( -3.987046614173229475, 3.845309131478920506, 8.397573164612470720 ) ) ;
#5772 = ORIENTED_EDGE ( 'NONE', *, *, #3974, .F. ) ;
#5773 = DIRECTION ( 'NONE',  ( -1.000000000000000000, -0.000000000000000000, -0.000000000000000000 ) ) ;
#5774 = CC_DESIGN_DATE_AND_TIME_ASSIGNMENT ( #2100, #7749, ( #1914 ) ) ;
#5775 = FACE_OUTER_BOUND ( 'NONE', #2874, .T. ) ;
#5776 = APPLICATION_PROTOCOL_DEFINITION ( 'international standard', 'config_control_design', 1994, #1684 ) ;
#5777 = ORIENTED_EDGE ( 'NONE', *, *, #4375, .T. ) ;
#5778 = ADVANCED_FACE ( 'NONE', ( #865 ), #3364, .T. ) ;
#5779 = LINE ( 'NONE', #2008, #4761 ) ;
#5780 = FACE_OUTER_BOUND ( 'NONE', #4975, .T. ) ;
#5781 = PLANE ( 'NONE',  #1110 ) ;
#5782 = EDGE_LOOP ( 'NONE', ( #5705, #2014 ) ) ;
#5783 = DIRECTION ( 'NONE',  ( -0.1278538906451907875, 0.000000000000000000, -0.9917930140139562534 ) ) ;
#5784 = ORIENTED_EDGE ( 'NONE', *, *, #4013, .T. ) ;
#5785 = ADVANCED_FACE ( 'NONE', ( #749, #3241 ), #116, .T. ) ;
#5786 = UNCERTAINTY_MEASURE_WITH_UNIT (LENGTH_MEASURE( 1.000000000000000082E-05 ), #7061, 'distance_accuracy_value', 'NONE');
#5787 = ADVANCED_FACE ( 'NONE', ( #7785 ), #373, .F. ) ;
#5788 = CARTESIAN_POINT ( 'NONE',  ( 3.987953385826774166, 3.853790179939030391, 8.059880408514990435 ) ) ;
#5789 = CARTESIAN_POINT ( 'NONE',  ( 0.4244988595014765331, 5.194936639113962862, -5.108750000000002345 ) ) ;
#5790 = DIRECTION ( 'NONE',  ( -1.000000000000000000, 0.000000000000000000, -0.000000000000000000 ) ) ;
#5791 = CARTESIAN_POINT ( 'NONE',  ( 3.987953385826772390, 3.876126805297290812, 8.413336896757332539 ) ) ;
#5792 = VERTEX_POINT ( 'NONE', #909 ) ;
#5793 = APPROVAL_PERSON_ORGANIZATION ( #5762, #7614, #4648 ) ;
#5794 =( BOUNDED_CURVE ( )  B_SPLINE_CURVE ( 3, ( #2913, #916, #1575, #8017 ),
 .UNSPECIFIED., .F., .T. ) 
 B_SPLINE_CURVE_WITH_KNOTS ( ( 4, 4 ),
 ( 1.387778780781445676E-17, 0.03896959987227040928 ),
 .UNSPECIFIED. ) 
 CURVE ( )  GEOMETRIC_REPRESENTATION_ITEM ( )  RATIONAL_B_SPLINE_CURVE ( ( 0.5972799528396773860, 0.6362002289060533222, 0.6867990768019666126, 0.7490764965274174791 ) ) 
 REPRESENTATION_ITEM ( '' )  );
#5795 = DIRECTION ( 'NONE',  ( -0.000000000000000000, -1.000000000000000000, -0.000000000000000000 ) ) ;
#5796 = CARTESIAN_POINT ( 'NONE',  ( 0.000000000000000000, 3.950000000000000178, 2.750000000000000888 ) ) ;
#5797 = VECTOR ( 'NONE', #6181, 39.37007874015748143 ) ;
#5798 = EDGE_LOOP ( 'NONE', ( #2128, #134, #1820, #5008 ) ) ;
#5799 = SHAPE_DEFINITION_REPRESENTATION ( #2672, #6925 ) ;
#5800 = VECTOR ( 'NONE', #7449, 39.37007874015748143 ) ;
#5801 = FACE_OUTER_BOUND ( 'NONE', #1885, .T. ) ;
#5802 = LOCAL_TIME ( 0, 37, 23.00000000000000000, #257 ) ;
#5803 = APPROVAL_DATE_TIME ( #4690, #4508 ) ;
#5804 = CARTESIAN_POINT ( 'NONE',  ( 3.874999998766638587, 1.000000000000000222, -3.894564048797845777E-16 ) ) ;
#5805 = CARTESIAN_POINT ( 'NONE',  ( 0.7371834602650290114, 4.089377917019955788, 8.511693372783511791 ) ) ;
#5806 = DIRECTION ( 'NONE',  ( 1.000000000000000000, 0.000000000000000000, -0.000000000000000000 ) ) ;
#5807 = CARTESIAN_POINT ( 'NONE',  ( 0.6820189411826722559, 3.637988102632602860, 8.251574762515335948 ) ) ;
#5808 = ADVANCED_FACE ( 'NONE', ( #2132 ), #4630, .F. ) ;
#5809 = AXIS2_PLACEMENT_3D ( 'NONE', #7891, #6083, #4102 ) ;
#5810 = VERTEX_POINT ( 'NONE', #455 ) ;
#5811 = CARTESIAN_POINT ( 'NONE',  ( -3.987046614173229919, 4.046209851938014523, 8.059880408515109451 ) ) ;
#5812 = CARTESIAN_POINT ( 'NONE',  ( -3.987046614173229475, 3.793298628414998763, 8.349863190998451756 ) ) ;
#5813 = VERTEX_POINT ( 'NONE', #1647 ) ;
#5814 = CARTESIAN_POINT ( 'NONE',  ( -3.987046614173228587, 4.225666661560477877, 8.231249998505111520 ) ) ;
#5815 = CARTESIAN_POINT ( 'NONE',  ( -1.475084850638524347, 9.463787071442423482, 8.576134714945274240 ) ) ;
#5816 = CARTESIAN_POINT ( 'NONE',  ( 2.750000000000000444, 7.531471846334603981, 3.944609322583843891 ) ) ;
#5817 = CARTESIAN_POINT ( 'NONE',  ( 0.000000000000000000, 3.950000000000000178, 8.981250000000001066 ) ) ;
#5818 = PERSON_AND_ORGANIZATION_ROLE ( 'creator' ) ;
#5819 = ORIENTED_EDGE ( 'NONE', *, *, #3023, .T. ) ;
#5820 = AXIS2_PLACEMENT_3D ( 'NONE', #1972, #1357, #3847 ) ;
#5821 = DIRECTION ( 'NONE',  ( 0.000000000000000000, 0.000000000000000000, -1.000000000000000000 ) ) ;
#5822 = CC_DESIGN_DATE_AND_TIME_ASSIGNMENT ( #4076, #990, ( #3381 ) ) ;
#5823 = CARTESIAN_POINT ( 'NONE',  ( -1.304290195246832873, 3.801843365448688505, -5.108750000000001457 ) ) ;
#5824 = DIRECTION ( 'NONE',  ( 0.000000000000000000, -1.000000000000000000, 0.000000000000000000 ) ) ;
#5825 = CARTESIAN_POINT ( 'NONE',  ( 2.750000000000000888, 8.589000000000000412, 3.243476614173229411 ) ) ;
#5826 =( CONVERSION_BASED_UNIT ( 'INCH', #3323 ) LENGTH_UNIT ( ) NAMED_UNIT ( #2615 ) );
#5827 = CARTESIAN_POINT ( 'NONE',  ( -8.751021560936518753E-10, 1.365923996832131609E-16, 5.750408897959578548E-10 ) ) ;
#5828 = EDGE_CURVE ( 'NONE', #2504, #7789, #6344, .T. ) ;
#5829 = COORDINATED_UNIVERSAL_TIME_OFFSET ( 0, 0, .AHEAD. ) ;
#5830 = ORIENTED_EDGE ( 'NONE', *, *, #1035, .T. ) ;
#5831 = CARTESIAN_POINT ( 'NONE',  ( 0.000000000000000000, 5.414000000000000590, 0.000000000000000000 ) ) ;
#5832 = CARTESIAN_POINT ( 'NONE',  ( 0.7499999999999995559, 3.929097005416127164, 8.543750000000002842 ) ) ;
#5833 = VECTOR ( 'NONE', #897, 39.37007874015748143 ) ;
#5834 = ORGANIZATION ( 'NAUO-ORG6', 'UNSPECIFIED', 'UNSPECIFIED' ) ;
#5835 = DIRECTION ( 'NONE',  ( -0.000000000000000000, -1.000000000000000000, -0.000000000000000000 ) ) ;
#5836 = AXIS2_PLACEMENT_3D ( 'NONE', #4350, #5007, #7431 ) ;
#5837 = CARTESIAN_POINT ( 'NONE',  ( 4.462953385826773811, 3.674333370316265945, 8.231249998505111520 ) ) ;
#5838 = DIRECTION ( 'NONE',  ( 0.000000000000000000, 0.000000000000000000, -1.000000000000000000 ) ) ;
#5839 = ADVANCED_FACE ( 'NONE', ( #5237 ), #7142, .F. ) ;
#5840 = EDGE_CURVE ( 'NONE', #4981, #7723, #2182, .T. ) ;
#5841 = ORIENTED_EDGE ( 'NONE', *, *, #3629, .T. ) ;
#5842 = VECTOR ( 'NONE', #5525, 39.37007874015748143 ) ;
#5843 = ADVANCED_FACE ( 'NONE', ( #5946 ), #1037, .T. ) ;
#5844 = AXIS2_PLACEMENT_3D ( 'NONE', #3045, #1791, #8113 ) ;
#5845 = LINE ( 'NONE', #3897, #3089 ) ;
#5846 = CARTESIAN_POINT ( 'NONE',  ( -2.749999999999999556, 8.589000000000000412, 3.161250000000001670 ) ) ;
#5847 = CIRCLE ( 'NONE', #873, 1.624999995942718156 ) ;
#5848 = ORIENTED_EDGE ( 'NONE', *, *, #2686, .T. ) ;
#5849 = EDGE_CURVE ( 'NONE', #4298, #4397, #5904, .T. ) ;
#5850 = CIRCLE ( 'NONE', #7848, 4.805751768934915624 ) ;
#5851 = DATE_AND_TIME ( #2113, #3576 ) ;
#5852 = CARTESIAN_POINT ( 'NONE',  ( -1.388463899750249738E-31, 3.950000000000000178, -4.043750000000001066 ) ) ;
#5853 = PERSON_AND_ORGANIZATION_ROLE ( 'classification_officer' ) ;
#5854 = CARTESIAN_POINT ( 'NONE',  ( 0.7274884641267198582, 3.767418641134389290, 7.977431595376885731 ) ) ;
#5855 = CARTESIAN_POINT ( 'NONE',  ( 0.7499999999999992228, 3.970895372960746350, 8.543750000000002842 ) ) ;
#5856 = VECTOR ( 'NONE', #7045, 39.37007874015748854 ) ;
#5857 = AXIS2_PLACEMENT_3D ( 'NONE', #1951, #4442, #3823 ) ;
#5858 = VERTEX_POINT ( 'NONE', #4047 ) ;
#5859 = DIRECTION ( 'NONE',  ( 0.000000000000000000, 0.000000000000000000, 1.000000000000000000 ) ) ;
#5860 = CARTESIAN_POINT ( 'NONE',  ( -3.987046614173229475, 3.787345657127929588, 8.341552593656997416 ) ) ;
#5861 = ORIENTED_EDGE ( 'NONE', *, *, #5333, .T. ) ;
#5862 = CARTESIAN_POINT ( 'NONE',  ( 0.000000000000000000, 5.025000000000000355, 3.440250000000001140 ) ) ;
#5863 = DIRECTION ( 'NONE',  ( 0.000000000000000000, -0.000000000000000000, 1.000000000000000000 ) ) ;
#5864 = LINE ( 'NONE', #2743, #6124 ) ;
#5865 = DATE_AND_TIME ( #3314, #8159 ) ;
#5866 = CIRCLE ( 'NONE', #1545, 0.1875000000000006661 ) ;
#5867 = ORIENTED_EDGE ( 'NONE', *, *, #7157, .F. ) ;
#5868 = CARTESIAN_POINT ( 'NONE',  ( 0.000000000000000000, 5.238734212598425977, 3.956250000000001155 ) ) ;
#5869 = DIRECTION ( 'NONE',  ( -0.000000000000000000, 1.000000000000000000, -0.000000000000000000 ) ) ;
#5870 = SHAPE_REPRESENTATION_RELATIONSHIP ( 'NONE' , 'NONE' ,  #6505, #5441 ) ;
#5871 = CARTESIAN_POINT ( 'NONE',  ( 2.750000000000000444, 7.964000000000000412, 3.823750000000002647 ) ) ;
#5872 = ORIENTED_EDGE ( 'NONE', *, *, #1683, .F. ) ;
#5873 = DATE_AND_TIME ( #5906, #2149 ) ;
#5874 = ORIENTED_EDGE ( 'NONE', *, *, #6299, .T. ) ;
#5875 = DIRECTION ( 'NONE',  ( 0.000000000000000000, -0.9090648228942841413, -0.4166547104932138423 ) ) ;
#5876 = CARTESIAN_POINT ( 'NONE',  ( 3.987953385826774166, 3.756917219824144283, 8.194756059061692355 ) ) ;
#5877 = LINE ( 'NONE', #6001, #7941 ) ;
#5878 = CARTESIAN_POINT ( 'NONE',  ( -1.187499999717754884, 7.436775081331068016, 4.083473622121677415 ) ) ;
#5879 = CC_DESIGN_DATE_AND_TIME_ASSIGNMENT ( #4447, #1800, ( #7802 ) ) ;
#5880 = CARTESIAN_POINT ( 'NONE',  ( 3.987953385826772390, 4.145406495827570481, 8.255194476359251965 ) ) ;
#5881 = EDGE_LOOP ( 'NONE', ( #7498, #6806, #7624, #6960 ) ) ;
#5882 = PRODUCT_DEFINITION_SHAPE ( 'NONE', 'NONE',  #8193 ) ;
#5883 = DIRECTION ( 'NONE',  ( 0.000000000000000000, 1.000000000000000000, 0.000000000000000000 ) ) ;
#5884 = CARTESIAN_POINT ( 'NONE',  ( -2.740000000000000213, 8.729000000000002757, 3.823750000000002647 ) ) ;
#5885 = DATE_TIME_ROLE ( 'creation_date' ) ;
#5886 = EDGE_CURVE ( 'NONE', #7545, #6458, #6232, .T. ) ;
#5887 = CARTESIAN_POINT ( 'NONE',  ( 2.750000000000000444, 7.964000000000001300, 3.691250000000001030 ) ) ;
#5888 = COORDINATED_UNIVERSAL_TIME_OFFSET ( 0, 0, .AHEAD. ) ;
#5889 = CARTESIAN_POINT ( 'NONE',  ( -2.750000000000000888, 7.974000000000001087, 3.813750000000002416 ) ) ;
#5890 = PLANE ( 'NONE',  #1537 ) ;
#5891 = ORIENTED_EDGE ( 'NONE', *, *, #4278, .T. ) ;
#5892 = CARTESIAN_POINT ( 'NONE',  ( -3.121988307086614345, 2.389005866141732604, 4.968462007874016706 ) ) ;
#5893 = CARTESIAN_POINT ( 'NONE',  ( -3.987046614173228143, 3.999111350888635563, 8.423148454254917539 ) ) ;
#5894 = VERTEX_POINT ( 'NONE', #1689 ) ;
#5895 = CARTESIAN_POINT ( 'NONE',  ( -2.577468385826771957, 2.661265787401575267, 3.956250000000000266 ) ) ;
#5896 = ORIENTED_EDGE ( 'NONE', *, *, #879, .F. ) ;
#5897 = FACE_OUTER_BOUND ( 'NONE', #222, .T. ) ;
#5898 = PERSON_AND_ORGANIZATION ( #7862, #8117 ) ;
#5899 = VERTEX_POINT ( 'NONE', #3564 ) ;
#5900 = LOCAL_TIME ( 0, 37, 23.00000000000000000, #5573 ) ;
#5901 = EDGE_CURVE ( 'NONE', #5688, #4355, #2904, .T. ) ;
#5902 = CARTESIAN_POINT ( 'NONE',  ( -0.8990231271313871009, 2.992770062582230661, -5.108749999999997904 ) ) ;
#5903 = PLANE ( 'NONE',  #4628 ) ;
#5904 = LINE ( 'NONE', #292, #179 ) ;
#5905 = ORIENTED_EDGE ( 'NONE', *, *, #5507, .T. ) ;
#5906 = CALENDAR_DATE ( 2026, 8, 10 ) ;
#5907 = ORIENTED_EDGE ( 'NONE', *, *, #2898, .T. ) ;
#5908 = CARTESIAN_POINT ( 'NONE',  ( 0.6829499219002717059, 3.640031188008940433, 8.272284810380444497 ) ) ;
#5909 = DIRECTION ( 'NONE',  ( 0.000000000000000000, -0.7071067811865474617, 0.7071067811865474617 ) ) ;
#5910 = CARTESIAN_POINT ( 'NONE',  ( 3.987953385826771946, 3.674333370316265501, 7.679916707260901809 ) ) ;
#5911 = DIRECTION ( 'NONE',  ( -0.000000000000000000, -0.000000000000000000, -1.000000000000000000 ) ) ;
#5912 = CARTESIAN_POINT ( 'NONE',  ( 3.987953385826772834, 4.142924502496692085, 8.268572589389476590 ) ) ;
#5913 =( BOUNDED_CURVE ( )  B_SPLINE_CURVE ( 2, ( #4881, #504, #8101, #3623, #6662, #5408, #4926, #4214, #7368 ),
 .UNSPECIFIED., .F., .T. ) 
 B_SPLINE_CURVE_WITH_KNOTS ( ( 3, 2, 2, 2, 3 ),
 ( 8.057829014928736820E-13, 0.01376350590615705097, 0.04131120849338899143, 0.06885891108062074106, 0.07294458655603817954 ),
 .UNSPECIFIED. ) 
 CURVE ( )  GEOMETRIC_REPRESENTATION_ITEM ( )  RATIONAL_B_SPLINE_CURVE ( ( 0.8535534732088591037, 0.8536633850130399548, 1.000000000000000000, 0.7071067811865479058, 1.000000000000000000, 0.7071067811865479058, 1.000000000000000000, 0.9565602018087399072, 0.9260057553135141450 ) ) 
 REPRESENTATION_ITEM ( '' )  );
#5914 = VERTEX_POINT ( 'NONE', #2832 ) ;
#5915 = PRODUCT_RELATED_PRODUCT_CATEGORY ( 'detail', '', ( #4489 ) ) ;
#5916 = DIRECTION ( 'NONE',  ( 1.000000000000000000, 0.000000000000000000, 0.000000000000000000 ) ) ;
#5917 = CARTESIAN_POINT ( 'NONE',  ( 0.000000000000000000, 3.950000000000000178, 3.691250000234376216 ) ) ;
#5918 = DIRECTION ( 'NONE',  ( -0.000000000000000000, -0.000000000000000000, 1.000000000000000000 ) ) ;
#5919 = PERSON_AND_ORGANIZATION ( #7862, #8117 ) ;
#5920 = CARTESIAN_POINT ( 'NONE',  ( 1.124999999999999556, 3.950000000000000178, 6.956250000000000711 ) ) ;
#5921 = ADVANCED_FACE ( 'NONE', ( #7833 ), #4759, .T. ) ;
#5922 = PERSON_AND_ORGANIZATION_ROLE ( 'classification_officer' ) ;
#5923 = DIRECTION ( 'NONE',  ( -0.000000000000000000, 0.000000000000000000, -1.000000000000000000 ) ) ;
#5924 = CARTESIAN_POINT ( 'NONE',  ( 0.7466433925744946354, 4.021593608141584397, 8.535611635381275875 ) ) ;
#5925 = FACE_OUTER_BOUND ( 'NONE', #3674, .T. ) ;
#5926 = CC_DESIGN_SECURITY_CLASSIFICATION ( #3944, ( #7291 ) ) ;
#5927 = ORIENTED_EDGE ( 'NONE', *, *, #6989, .F. ) ;
#5928 = VECTOR ( 'NONE', #7371, 39.37007874015748143 ) ;
#5929 = CARTESIAN_POINT ( 'NONE',  ( -2.852014645669292303, 5.376007322834644775, 5.972081456692913015 ) ) ;
#5930 = VECTOR ( 'NONE', #6742, 39.37007874015748143 ) ;
#5931 = LOCAL_TIME ( 0, 37, 23.00000000000000000, #3635 ) ;
#5932 = DIRECTION ( 'NONE',  ( 1.000000000000000000, -0.000000000000000000, 0.000000000000000000 ) ) ;
#5933 = ORIENTED_EDGE ( 'NONE', *, *, #7643, .F. ) ;
#5934 = CARTESIAN_POINT ( 'NONE',  ( 1.625000000000000222, 2.500000000000000000, -2.521780125229002412 ) ) ;
#5935 = ORIENTED_EDGE ( 'NONE', *, *, #2836, .F. ) ;
#5936 = DIRECTION ( 'NONE',  ( -0.000000000000000000, -1.000000000000000000, -0.000000000000000000 ) ) ;
#5937 = PERSON_AND_ORGANIZATION_ROLE ( 'design_supplier' ) ;
#5938 = ORIENTED_EDGE ( 'NONE', *, *, #6042, .F. ) ;
#5939 = ADVANCED_FACE ( 'NONE', ( #5520 ), #3072, .T. ) ;
#5940 = AXIS2_PLACEMENT_3D ( 'NONE', #103, #1959, #5070 ) ;
#5941 = PRODUCT_DEFINITION_FORMATION_WITH_SPECIFIED_SOURCE ( 'ANY', '', #3896, .NOT_KNOWN. ) ;
#5942 = EDGE_CURVE ( 'NONE', #3004, #1632, #7495, .T. ) ;
#5943 = CARTESIAN_POINT ( 'NONE',  ( -0.9907400750648208687, 3.084787739353607172, -5.108749999999999680 ) ) ;
#5944 = DIRECTION ( 'NONE',  ( 0.000000000000000000, -0.000000000000000000, 1.000000000000000000 ) ) ;
#5945 = VECTOR ( 'NONE', #496, 39.37007874015748143 ) ;
#5946 = FACE_OUTER_BOUND ( 'NONE', #2765, .T. ) ;
#5947 = COORDINATED_UNIVERSAL_TIME_OFFSET ( 0, 0, .AHEAD. ) ;
#5948 = ADVANCED_FACE ( 'NONE', ( #2384 ), #6768, .F. ) ;
#5949 = EDGE_LOOP ( 'NONE', ( #465, #1713, #4123, #1138 ) ) ;
#5950 = AXIS2_PLACEMENT_3D ( 'NONE', #1408, #5702, #1321 ) ;
#5951 = UNCERTAINTY_MEASURE_WITH_UNIT (LENGTH_MEASURE( 1.000000000000000082E-05 ), #5359, 'distance_accuracy_value', 'NONE');
#5952 = AXIS2_PLACEMENT_3D ( 'NONE', #4324, #2893, #6826 ) ;
#5953 = LINE ( 'NONE', #336, #574 ) ;
#5954 = CARTESIAN_POINT ( 'NONE',  ( 0.000000000000000000, 3.950000000000000178, 7.131250000000001421 ) ) ;
#5955 = VECTOR ( 'NONE', #2982, 39.37007874015748143 ) ;
#5956 = DIRECTION ( 'NONE',  ( 0.000000000000000000, 0.000000000000000000, -1.000000000000000000 ) ) ;
#5957 = EDGE_CURVE ( 'NONE', #3479, #5810, #5079, .T. ) ;
#5958 = CARTESIAN_POINT ( 'NONE',  ( 3.987953385826771946, 4.142138515950337663, 8.272475195627956523 ) ) ;
#5959 = AXIS2_PLACEMENT_3D ( 'NONE', #2091, #4581, #7090 ) ;
#5960 = ORIENTED_EDGE ( 'NONE', *, *, #1584, .T. ) ;
#5961 = CIRCLE ( 'NONE', #7704, 2.841000000000000636 ) ;
#5962 = APPROVAL_PERSON_ORGANIZATION ( #7996, #2224, #5432 ) ;
#5963 = FACE_BOUND ( 'NONE', #7178, .T. ) ;
#5964 = LINE ( 'NONE', #1621, #1270 ) ;
#5965 = CARTESIAN_POINT ( 'NONE',  ( 0.4157371843214867635, 2.378754802131286095, -3.027323041911860635 ) ) ;
#5966 = LINE ( 'NONE', #2111, #6626 ) ;
#5967 = DIRECTION ( 'NONE',  ( 0.000000000000000000, -1.000000000000000000, 0.000000000000000000 ) ) ;
#5968 = EDGE_LOOP ( 'NONE', ( #2565, #6564 ) ) ;
#5969 = CALENDAR_DATE ( 2026, 8, 10 ) ;
#5970 = FACE_OUTER_BOUND ( 'NONE', #4941, .T. ) ;
#5971 = VECTOR ( 'NONE', #8026, 39.37007874015748143 ) ;
#5972 = CC_DESIGN_PERSON_AND_ORGANIZATION_ASSIGNMENT ( #3110, #3829, ( #1242 ) ) ;
#5973 = CARTESIAN_POINT ( 'NONE',  ( 0.6994737761126073039, 4.220893194183548580, 8.388378218819653398 ) ) ;
#5974 = ORIENTED_EDGE ( 'NONE', *, *, #589, .F. ) ;
#5975 = APPLICATION_CONTEXT ( 'configuration controlled 3d designs of mechanical parts and assemblies' ) ;
#5976 = DIRECTION ( 'NONE',  ( -1.000000000000000000, 0.000000000000000000, -0.000000000000000000 ) ) ;
#5977 = AXIS2_PLACEMENT_3D ( 'NONE', #7851, #5294, #3462 ) ;
#5978 = ORIENTED_EDGE ( 'NONE', *, *, #1955, .F. ) ;
#5979 = DIRECTION ( 'NONE',  ( 0.08785522444269371067, 0.000000000000000000, 0.9961332539063856295 ) ) ;
#5980 = LINE ( 'NONE', #7945, #3494 ) ;
#5981 = VERTEX_POINT ( 'NONE', #2952 ) ;
#5982 = PERSON_AND_ORGANIZATION_ROLE ( 'design_owner' ) ;
#5983 = FACE_BOUND ( 'NONE', #3895, .T. ) ;
#5984 = APPROVAL_STATUS ( 'not_yet_approved' ) ;
#5985 = ORIENTED_EDGE ( 'NONE', *, *, #3956, .T. ) ;
#5986 = CC_DESIGN_DATE_AND_TIME_ASSIGNMENT ( #4606, #5885, ( #2483 ) ) ;
#5987 = CARTESIAN_POINT ( 'NONE',  ( -1.187500000000000222, 7.339000000000003077, 5.236250000000000959 ) ) ;
#5988 = AXIS2_PLACEMENT_3D ( 'NONE', #1712, #4238, #5468 ) ;
#5989 = AXIS2_PLACEMENT_3D ( 'NONE', #6256, #6868, #1259 ) ;
#5990 = CARTESIAN_POINT ( 'NONE',  ( -0.5830436547479556086, 2.773322901827991682, -5.108750000000002345 ) ) ;
#5991 = CARTESIAN_POINT ( 'NONE',  ( 0.5362929982961579523, 2.415731535078691206, 2.991079242820094297 ) ) ;
#5992 = LINE ( 'NONE', #3361, #4371 ) ;
#5993 = AXIS2_PLACEMENT_3D ( 'NONE', #3870, #685, #649 ) ;
#5994 = VECTOR ( 'NONE', #5736, 39.37007874015748854 ) ;
#5995 = CARTESIAN_POINT ( 'NONE',  ( -1.312500000000000888, 7.964000000000000412, 2.411250000000000338 ) ) ;
#5996 = CALENDAR_DATE ( 2026, 8, 10 ) ;
#5997 = ORIENTED_EDGE ( 'NONE', *, *, #3251, .F. ) ;
#5998 = EDGE_CURVE ( 'NONE', #5062, #1711, #2552, .T. ) ;
#5999 = CARTESIAN_POINT ( 'NONE',  ( -3.362500000000001155, 1.750000000000000444, 4.117874862132976456E-16 ) ) ;
#6000 = CARTESIAN_POINT ( 'NONE',  ( 4.470366332363715500, 1.365923996832131609E-16, 2.937534001674281914 ) ) ;
#6001 = CARTESIAN_POINT ( 'NONE',  ( 0.000000000000000000, 8.574153543307087233, 3.323750000000000870 ) ) ;
#6002 = CARTESIAN_POINT ( 'NONE',  ( 2.349999998660270872, 3.550000000000001155, -1.169467086614173645 ) ) ;
#6003 = VERTEX_POINT ( 'NONE', #2344 ) ;
#6004 = CARTESIAN_POINT ( 'NONE',  ( -3.987046614173229475, 4.123102181196484750, 8.137838423722035586 ) ) ;
#6005 = CARTESIAN_POINT ( 'NONE',  ( -3.687499989627468722, 1.365923996832131609E-16, 3.874999999790588401 ) ) ;
#6006 = PLANE ( 'NONE',  #7815 ) ;
#6007 = ORIENTED_EDGE ( 'NONE', *, *, #1970, .T. ) ;
#6008 = SECURITY_CLASSIFICATION_LEVEL ( 'unclassified' ) ;
#6009 = DIRECTION ( 'NONE',  ( 0.9961332539063856295, 0.000000000000000000, -0.08785522444269552866 ) ) ;
#6010 = CARTESIAN_POINT ( 'NONE',  ( 0.6817881100752513079, 4.262513956817777228, 8.221358888732334336 ) ) ;
#6011 = FACE_OUTER_BOUND ( 'NONE', #5550, .T. ) ;
#6012 = ORIENTED_EDGE ( 'NONE', *, *, #6084, .F. ) ;
#6013 = CARTESIAN_POINT ( 'NONE',  ( -3.874999999933440797, 1.000000000000000222, -5.476399496138180442E-16 ) ) ;
#6014 = PLANE ( 'NONE',  #1644 ) ;
#6015 = CARTESIAN_POINT ( 'NONE',  ( 0.000000000000000000, 5.024999999999999467, 3.742515787401575533 ) ) ;
#6016 = EDGE_LOOP ( 'NONE', ( #7799, #2843, #3293 ) ) ;
#6017 = APPROVAL_DATE_TIME ( #3520, #7190 ) ;
#6018 =( BOUNDED_CURVE ( )  B_SPLINE_CURVE ( 2, ( #2771, #1018, #1057, #3514, #3593, #4151, #6092 ),
 .UNSPECIFIED., .F., .F. ) 
 B_SPLINE_CURVE_WITH_KNOTS ( ( 3, 2, 2, 3 ),
 ( 1.018141215013587730E-11, 0.003869794778861493714, 0.03119827453828998703, 0.05852675429817026653 ),
 .UNSPECIFIED. ) 
 CURVE ( )  GEOMETRIC_REPRESENTATION_ITEM ( )  RATIONAL_B_SPLINE_CURVE ( ( 0.9287967261194141066, 0.9585254410079242504, 1.000000000000000000, 0.7071067811865479058, 1.000000000000000000, 0.7071067811865479058, 1.000000000000000000 ) ) 
 REPRESENTATION_ITEM ( '' )  );
#6019 = FACE_OUTER_BOUND ( 'NONE', #1437, .T. ) ;
#6020 = DIRECTION ( 'NONE',  ( 0.000000000000000000, 0.000000000000000000, 1.000000000000000000 ) ) ;
#6021 = DATE_TIME_ROLE ( 'classification_date' ) ;
#6022 = ORIENTED_EDGE ( 'NONE', *, *, #1642, .F. ) ;
#6023 = LINE ( 'NONE', #408, #480 ) ;
#6024 = APPLICATION_CONTEXT ( 'configuration controlled 3d designs of mechanical parts and assemblies' ) ;
#6025 = LINE ( 'NONE', #2902, #25 ) ;
#6026 = CARTESIAN_POINT ( 'NONE',  ( -0.6238927636269362420, 2.448270400771923594, 2.959268117001225384 ) ) ;
#6027 = PRODUCT_RELATED_PRODUCT_CATEGORY ( 'detail', '', ( #3896 ) ) ;
#6028 = DIRECTION ( 'NONE',  ( 0.000000000000000000, 1.000000000000000000, -0.000000000000000000 ) ) ;
#6029 = CARTESIAN_POINT ( 'NONE',  ( -2.750000000000000444, 7.338999999999999524, 3.471636850393701401 ) ) ;
#6030 = CC_DESIGN_SECURITY_CLASSIFICATION ( #1058, ( #8198 ) ) ;
#6031 = CARTESIAN_POINT ( 'NONE',  ( -1.312500000000000444, 7.339000000000003077, 2.411250000000000782 ) ) ;
#6032 = APPLICATION_PROTOCOL_DEFINITION ( 'international standard', 'config_control_design', 1994, #6024 ) ;
#6033 = ORGANIZATION ( 'NAUO-ORG1', 'UNSPECIFIED', 'UNSPECIFIED' ) ;
#6034 = ORIENTED_EDGE ( 'NONE', *, *, #239, .F. ) ;
#6035 = CARTESIAN_POINT ( 'NONE',  ( -2.750000000000000444, 7.521783346456694552, 3.956250000000000266 ) ) ;
#6036 = EDGE_CURVE ( 'NONE', #1469, #2357, #7824, .T. ) ;
#6037 = DESIGN_CONTEXT ( 'detailed design', #5975, 'design' ) ;
#6038 = CARTESIAN_POINT ( 'NONE',  ( 1.187500002638678165, 4.186788052716939212, 6.858307716535433585 ) ) ;
#6039 = CARTESIAN_POINT ( 'NONE',  ( 0.000000000000000000, 3.950000000000000178, 8.831250000000000711 ) ) ;
#6040 = SHAPE_REPRESENTATION ( 'bench vise6_2-', ( #7272 ), #588 ) ;
#6041 = DIRECTION ( 'NONE',  ( -0.000000000000000000, 1.000000000000000000, -0.000000000000000000 ) ) ;
#6042 = EDGE_CURVE ( 'NONE', #6680, #5712, #8134, .T. ) ;
#6043 = ORIENTED_EDGE ( 'NONE', *, *, #2920, .F. ) ;
#6044 = EDGE_CURVE ( 'NONE', #7058, #5792, #1239, .T. ) ;
#6045 = CARTESIAN_POINT ( 'NONE',  ( -3.987046614173228587, 4.012112954394242870, 8.044773094730338414 ) ) ;
#6046 = DIRECTION ( 'NONE',  ( -0.000000000000000000, -1.000000000000000000, -0.000000000000000000 ) ) ;
#6047 = DIRECTION ( 'NONE',  ( 0.7071067811865474617, 0.000000000000000000, 0.7071067811865474617 ) ) ;
#6048 = VERTEX_POINT ( 'NONE', #6724 ) ;
#6049 = PERSON_AND_ORGANIZATION ( #7862, #8117 ) ;
#6050 = LINE ( 'NONE', #6133, #7437 ) ;
#6051 = ORIENTED_EDGE ( 'NONE', *, *, #1778, .T. ) ;
#6052 = ORIENTED_EDGE ( 'NONE', *, *, #5576, .T. ) ;
#6053 = DIRECTION ( 'NONE',  ( 0.000000000000000000, 0.000000000000000000, -1.000000000000000000 ) ) ;
#6054 = CARTESIAN_POINT ( 'NONE',  ( -1.187500000000000222, 5.969165905511811587, 6.858307716535433585 ) ) ;
#6055 = VERTEX_POINT ( 'NONE', #6110 ) ;
#6056 = APPROVAL_DATE_TIME ( #5349, #2224 ) ;
#6057 = CARTESIAN_POINT ( 'NONE',  ( 4.383786719160104539, 4.383999996532199184, 8.231249998505111520 ) ) ;
#6058 = COORDINATED_UNIVERSAL_TIME_OFFSET ( 0, 0, .AHEAD. ) ;
#6059 = EDGE_CURVE ( 'NONE', #1840, #1442, #2432, .T. ) ;
#6060 = EDGE_LOOP ( 'NONE', ( #2922, #5471, #2311 ) ) ;
#6061 = VECTOR ( 'NONE', #1735, 39.37007874015748143 ) ;
#6062 = AXIS2_PLACEMENT_3D ( 'NONE', #4276, #6811, #8054 ) ;
#6063 = APPROVAL_PERSON_ORGANIZATION ( #272, #4518, #2766 ) ;
#6064 = DIRECTION ( 'NONE',  ( 0.000000000000000000, 0.000000000000000000, -1.000000000000000000 ) ) ;
#6065 = CARTESIAN_POINT ( 'NONE',  ( -4.382879947506562068, 4.383999996532200960, 8.231249998505111520 ) ) ;
#6066 = CARTESIAN_POINT ( 'NONE',  ( -0.7122575715994515777, 4.185397438661337510, 8.437773039678205578 ) ) ;
#6067 = DIRECTION ( 'NONE',  ( -0.000000000000000000, -1.000000000000000000, -0.000000000000000000 ) ) ;
#6068 = APPROVAL_STATUS ( 'not_yet_approved' ) ;
#6069 = ORIENTED_EDGE ( 'NONE', *, *, #1876, .T. ) ;
#6070 = VECTOR ( 'NONE', #667, 39.37007874015748143 ) ;
#6071 = CARTESIAN_POINT ( 'NONE',  ( -4.462046614173229564, 3.753500037801647871, 7.838250042231664771 ) ) ;
#6072 = APPROVAL ( #6134, 'UNKNOWN' ) ;
#6073 = AXIS2_PLACEMENT_3D ( 'NONE', #4496, #5111, #7650 ) ;
#6074 = CARTESIAN_POINT ( 'NONE',  ( 2.537500000000000533, 4.049999999999999822, 0.000000000000000000 ) ) ;
#6075 = CARTESIAN_POINT ( 'NONE',  ( -1.172489671586611548, 1.000000000000000888, -3.693357951819908891 ) ) ;
#6076 = DIRECTION ( 'NONE',  ( -0.7071067811865442421, 0.000000000000000000, -0.7071067811865507924 ) ) ;
#6077 = ORIENTED_EDGE ( 'NONE', *, *, #4126, .F. ) ;
#6078 = LINE ( 'NONE', #4140, #2259 ) ;
#6079 = ORIENTED_EDGE ( 'NONE', *, *, #337, .T. ) ;
#6080 = AXIS2_PLACEMENT_3D ( 'NONE', #885, #3384, #269 ) ;
#6081 = APPLICATION_CONTEXT ( 'configuration controlled 3d designs of mechanical parts and assemblies' ) ;
#6082 = VECTOR ( 'NONE', #7651, 39.37007874015748143 ) ;
#6083 = DIRECTION ( 'NONE',  ( 0.000000000000000000, 0.000000000000000000, -1.000000000000000000 ) ) ;
#6084 = EDGE_CURVE ( 'NONE', #1366, #3177, #7026, .T. ) ;
#6085 = DIRECTION ( 'NONE',  ( 0.000000000000000000, 0.000000000000000000, 1.000000000000000000 ) ) ;
#6086 = AXIS2_PLACEMENT_3D ( 'NONE', #1383, #761, #4979 ) ;
#6087 = LINE ( 'NONE', #472, #1354 ) ;
#6088 = LINE ( 'NONE', #2269, #447 ) ;
#6089 = EDGE_LOOP ( 'NONE', ( #998, #4479, #7252, #6738 ) ) ;
#6090 = PERSON_AND_ORGANIZATION ( #7862, #8117 ) ;
#6091 = CARTESIAN_POINT ( 'NONE',  ( 0.000000000000000000, 2.500000000000000000, 2.749999999536767437 ) ) ;
#6092 = CARTESIAN_POINT ( 'NONE',  ( 1.312500000000000444, 8.589000000000002188, 3.161250000147724837 ) ) ;
#6093 = EDGE_CURVE ( 'NONE', #6966, #3375, #6230, .T. ) ;
#6094 = AXIS2_PLACEMENT_3D ( 'NONE', #1265, #1869, #5678 ) ;
#6095 = ORGANIZATION ( 'NAUO-ORG9', 'UNSPECIFIED', 'UNSPECIFIED' ) ;
#6096 = ORIENTED_EDGE ( 'NONE', *, *, #3139, .F. ) ;
#6097 = CARTESIAN_POINT ( 'NONE',  ( -2.740000000000001545, 7.964000000000000412, 4.313750000000002416 ) ) ;
#6098 = LINE ( 'NONE', #5469, #7967 ) ;
#6099 = CARTESIAN_POINT ( 'NONE',  ( -2.740000000000001545, 8.719000000000002970, 3.823750000000002647 ) ) ;
#6100 = ORIENTED_EDGE ( 'NONE', *, *, #7364, .T. ) ;
#6101 = VECTOR ( 'NONE', #831, 39.37007874015748854 ) ;
#6102 = CALENDAR_DATE ( 2026, 8, 10 ) ;
#6103 = LINE ( 'NONE', #608, #7965 ) ;
#6104 = ITEM_DEFINED_TRANSFORMATION ( 'NONE', 'NONE', #6745,  #7272 ) ;
#6105 = ORIENTED_EDGE ( 'NONE', *, *, #6413, .T. ) ;
#6106 = CARTESIAN_POINT ( 'NONE',  ( 0.000000000000000000, 5.414000000000000590, 0.1249999999999999029 ) ) ;
#6107 = CARTESIAN_POINT ( 'NONE',  ( -2.753607252840604147, 0.9999999999981570298, -2.731109880590406824 ) ) ;
#6108 = DIRECTION ( 'NONE',  ( 0.000000000000000000, -0.000000000000000000, 1.000000000000000000 ) ) ;
#6109 = DIRECTION ( 'NONE',  ( -0.3026345437601031807, 0.000000000000000000, -0.9531066744720204653 ) ) ;
#6110 = CARTESIAN_POINT ( 'NONE',  ( 2.750000000000000444, 7.964000000000001300, 3.323749999955704304 ) ) ;
#6111 = VECTOR ( 'NONE', #931, 39.37007874015748143 ) ;
#6112 = COORDINATED_UNIVERSAL_TIME_OFFSET ( 0, 0, .AHEAD. ) ;
#6113 = CIRCLE ( 'NONE', #4665, 5.349138356872925826 ) ;
#6114 = EDGE_LOOP ( 'NONE', ( #2424, #6995, #2603 ) ) ;
#6115 = CARTESIAN_POINT ( 'NONE',  ( 3.362500000000000711, 1.750000000000000444, -8.235749724265952913E-16 ) ) ;
#6116 = ORIENTED_EDGE ( 'NONE', *, *, #4730, .F. ) ;
#6117 = CIRCLE ( 'NONE', #2587, 0.3625000012227142521 ) ;
#6118 = CARTESIAN_POINT ( 'NONE',  ( -1.625000000000000222, 3.950000000000000178, -2.750000000000000444 ) ) ;
#6119 = CARTESIAN_POINT ( 'NONE',  ( -2.875000000000000888, -3.820994292482255198E-18, -3.337500001222715174 ) ) ;
#6120 = ORIENTED_EDGE ( 'NONE', *, *, #6137, .F. ) ;
#6121 = FACE_OUTER_BOUND ( 'NONE', #6465, .T. ) ;
#6122 = EDGE_LOOP ( 'NONE', ( #6197, #5723, #3970, #2895 ) ) ;
#6123 = EDGE_CURVE ( 'NONE', #1507, #5196, #618, .T. ) ;
#6124 = VECTOR ( 'NONE', #1350, 39.37007874015748143 ) ;
#6125 = CARTESIAN_POINT ( 'NONE',  ( 2.946793808523474834, 2.500000000017352786, -0.5625000000000002220 ) ) ;
#6126 = CC_DESIGN_PERSON_AND_ORGANIZATION_ASSIGNMENT ( #2529, #5063, ( #4347 ) ) ;
#6127 = CARTESIAN_POINT ( 'NONE',  ( 3.796513186599488776, 1.365923996832131609E-16, -2.946478861041413211 ) ) ;
#6128 = DIRECTION ( 'NONE',  ( 0.5773502691896152950, 0.5773502691896467143, -0.5773502691896152950 ) ) ;
#6129 = CARTESIAN_POINT ( 'NONE',  ( 1.187500000000000222, 4.210703569520497958, 6.838410229878999047 ) ) ;
#6130 = ORIENTED_EDGE ( 'NONE', *, *, #3353, .T. ) ;
#6132 = SHAPE_DEFINITION_REPRESENTATION ( #8039, #6969 ) ;
#6131 = LOCAL_TIME ( 0, 37, 23.00000000000000000, #6395 ) ;
#6133 = CARTESIAN_POINT ( 'NONE',  ( -1.500000000000000444, 5.639000000000001123, 0.1250000000000000278 ) ) ;
#6134 = APPROVAL_STATUS ( 'not_yet_approved' ) ;
#6135 = APPLICATION_CONTEXT ( 'configuration controlled 3d designs of mechanical parts and assemblies' ) ;
#6136 = ADVANCED_FACE ( 'NONE', ( #497 ), #2987, .T. ) ;
#6137 = EDGE_CURVE ( 'NONE', #3352, #6974, #530, .T. ) ;
#6138 = ORIENTED_EDGE ( 'NONE', *, *, #2933, .F. ) ;
#6139 = CARTESIAN_POINT ( 'NONE',  ( -4.382879947506561180, 3.516000035344543306, 7.363250037317454755 ) ) ;
#6140 = ORIENTED_EDGE ( 'NONE', *, *, #4183, .F. ) ;
#6141 = SHAPE_DEFINITION_REPRESENTATION ( #2433, #3256 ) ;
#6142 = CARTESIAN_POINT ( 'NONE',  ( 4.462953385826773811, 3.674333370316266389, 8.231249998505111520 ) ) ;
#6143 = APPROVAL_ROLE ( '' ) ;
#6144 = LINE ( 'NONE', #4911, #1917 ) ;
#6145 = LINE ( 'NONE', #1723, #4356 ) ;
#6146 = FACE_OUTER_BOUND ( 'NONE', #146, .T. ) ;
#6147 = ORIENTED_EDGE ( 'NONE', *, *, #5479, .T. ) ;
#6148 = DIRECTION ( 'NONE',  ( 1.000000000000000000, 0.000000000000000000, 0.000000000000000000 ) ) ;
#6149 = DIRECTION ( 'NONE',  ( 0.7071067811865474617, 0.000000000000000000, 0.7071067811865474617 ) ) ;
#6150 = PERSON_AND_ORGANIZATION ( #7862, #8117 ) ;
#6151 = VERTEX_POINT ( 'NONE', #8178 ) ;
#6152 = EDGE_CURVE ( 'NONE', #3177, #2515, #7879, .T. ) ;
#6153 = ADVANCED_FACE ( 'NONE', ( #5775 ), #150, .T. ) ;
#6154 = ORIENTED_EDGE ( 'NONE', *, *, #3929, .T. ) ;
#6155 = CARTESIAN_POINT ( 'NONE',  ( -2.537500000000000533, 2.500000000000000444, -0.000000000000000000 ) ) ;
#6156 = CARTESIAN_POINT ( 'NONE',  ( -3.343750000000001776, 1.750000000000000444, 3.383875000000000632 ) ) ;
#6157 = ORIENTED_EDGE ( 'NONE', *, *, #7921, .T. ) ;
#6158 = ORIENTED_EDGE ( 'NONE', *, *, #675, .F. ) ;
#6159 = ADVANCED_FACE ( 'NONE', ( #3232, #5076 ), #1730, .T. ) ;
#6160 = CC_DESIGN_SECURITY_CLASSIFICATION ( #3008, ( #8197 ) ) ;
#6161 = ORIENTED_EDGE ( 'NONE', *, *, #1163, .F. ) ;
#6162 = LINE ( 'NONE', #4889, #6070 ) ;
#6163 = CARTESIAN_POINT ( 'NONE',  ( -0.7335700379171464780, 2.500000000182677873, -2.750000000000000444 ) ) ;
#6164 = CYLINDRICAL_SURFACE ( 'NONE', #3587, 5.349138356872925826 ) ;
#6165 = CARTESIAN_POINT ( 'NONE',  ( 1.187500000000000000, 4.734434094721707176, 5.776092429115636584 ) ) ;
#6166 = ORIENTED_EDGE ( 'NONE', *, *, #4724, .T. ) ;
#6167 = PERSON_AND_ORGANIZATION ( #7862, #8117 ) ;
#6168 = FACE_OUTER_BOUND ( 'NONE', #6773, .T. ) ;
#6169 = CC_DESIGN_PERSON_AND_ORGANIZATION_ASSIGNMENT ( #3881, #4459, ( #2206 ) ) ;
#6170 = ORIENTED_EDGE ( 'NONE', *, *, #1381, .T. ) ;
#6171 = CARTESIAN_POINT ( 'NONE',  ( 3.343750000000002220, 1.750000000000000444, -0.5625000000000003331 ) ) ;
#6172 = DIRECTION ( 'NONE',  ( -1.000000000000000000, 0.000000000000000000, 0.000000000000000000 ) ) ;
#6173 = EDGE_LOOP ( 'NONE', ( #1530, #3713 ) ) ;
#6174 = COORDINATED_UNIVERSAL_TIME_OFFSET ( 0, 0, .AHEAD. ) ;
#6175 = DIRECTION ( 'NONE',  ( -1.000000000000000000, 0.000000000000000000, 0.000000000000000000 ) ) ;
#6176 = APPROVAL_STATUS ( 'not_yet_approved' ) ;
#6177 = CARTESIAN_POINT ( 'NONE',  ( -1.625000000000000222, 2.500000000000000000, 2.521780125229002412 ) ) ;
#6178 = CC_DESIGN_DATE_AND_TIME_ASSIGNMENT ( #403, #7947, ( #516 ) ) ;
#6179 = DIRECTION ( 'NONE',  ( 1.000000000000000000, 0.000000000000000000, -0.000000000000000000 ) ) ;
#6180 = DIRECTION ( 'NONE',  ( 0.000000000000000000, -0.7071067811865282549, 0.7071067811865667796 ) ) ;
#6181 = DIRECTION ( 'NONE',  ( 0.000000000000000000, 1.000000000000000000, 0.000000000000000000 ) ) ;
#6182 = ORIENTED_EDGE ( 'NONE', *, *, #333, .F. ) ;
#6183 = CARTESIAN_POINT ( 'NONE',  ( -0.7499999999999993339, 3.950000000000000178, 7.918749999999998401 ) ) ;
#6184 = CALENDAR_DATE ( 2026, 8, 10 ) ;
#6185 = ORIENTED_EDGE ( 'NONE', *, *, #2568, .T. ) ;
#6186 = LINE ( 'NONE', #4921, #7984 ) ;
#6187 = EDGE_CURVE ( 'NONE', #4355, #5130, #5193, .T. ) ;
#6188 = APPROVAL_PERSON_ORGANIZATION ( #7390, #6229, #6759 ) ;
#6189 = ORIENTED_EDGE ( 'NONE', *, *, #6835, .T. ) ;
#6190 = CARTESIAN_POINT ( 'NONE',  ( 0.000000000000000000, 5.414000000000000590, 0.000000000000000000 ) ) ;
#6191 = FACE_OUTER_BOUND ( 'NONE', #7305, .T. ) ;
#6192 = CIRCLE ( 'NONE', #3046, 3.000000000000000888 ) ;
#6193 = AXIS2_PLACEMENT_3D ( 'NONE', #2296, #4868, #2340 ) ;
#6194 = CARTESIAN_POINT ( 'NONE',  ( 2.537500000000000533, 4.049999999999999822, 0.000000000000000000 ) ) ;
#6195 = SECURITY_CLASSIFICATION ( '', '', #6008 ) ;
#6196 = ORIENTED_EDGE ( 'NONE', *, *, #7780, .F. ) ;
#6197 = ORIENTED_EDGE ( 'NONE', *, *, #1891, .T. ) ;
#6198 = CIRCLE ( 'NONE', #1751, 0.3625000000000019318 ) ;
#6199 = CC_DESIGN_SECURITY_CLASSIFICATION ( #7674, ( #1877 ) ) ;
#6200 = CARTESIAN_POINT ( 'NONE',  ( 3.987953385826773278, 4.133273763909712351, 8.160372747217021328 ) ) ;
#6201 = EDGE_CURVE ( 'NONE', #8045, #6815, #7739, .T. ) ;
#6202 = CIRCLE ( 'NONE', #5950, 0.7499999999999993339 ) ;
#6203 = CARTESIAN_POINT ( 'NONE',  ( 1.187499999999999778, 4.552120669721712254, 6.297178727289153954 ) ) ;
#6204 = ORIENTED_EDGE ( 'NONE', *, *, #1931, .T. ) ;
#6205 = APPLICATION_PROTOCOL_DEFINITION ( 'international standard', 'config_control_design', 1994, #7363 ) ;
#6206 = VECTOR ( 'NONE', #6362, 39.37007874015748143 ) ;
#6207 = CARTESIAN_POINT ( 'NONE',  ( -1.500000000000000444, 5.414000000000000590, 0.1249999999999999445 ) ) ;
#6208 = VECTOR ( 'NONE', #5266, 39.37007874015748143 ) ;
#6209 = CONICAL_SURFACE ( 'NONE', #2426, 0.7499999999999993339, 0.7853981633974437271 ) ;
#6210 = PLANE ( 'NONE',  #1665 ) ;
#6211 = FACE_OUTER_BOUND ( 'NONE', #1134, .T. ) ;
#6212 = ORIENTED_EDGE ( 'NONE', *, *, #8098, .T. ) ;
#6213 = PERSON_AND_ORGANIZATION_ROLE ( 'creator' ) ;
#6214 = APPROVAL ( #8038, 'UNKNOWN' ) ;
#6215 = CARTESIAN_POINT ( 'NONE',  ( 2.740000000000000657, 7.969000000000000306, 3.328750000000002096 ) ) ;
#6216 = DATE_TIME_ROLE ( 'classification_date' ) ;
#6217 = LOCAL_TIME ( 0, 37, 23.00000000000000000, #10 ) ;
#6218 = LINE ( 'NONE', #3111, #5056 ) ;
#6219 = DIRECTION ( 'NONE',  ( -0.000000000000000000, 1.000000000000000000, -0.000000000000000000 ) ) ;
#6220 = APPROVAL_PERSON_ORGANIZATION ( #2245, #7190, #2285 ) ;
#6221 = CC_DESIGN_SECURITY_CLASSIFICATION ( #5167, ( #8191 ) ) ;
#6222 = CARTESIAN_POINT ( 'NONE',  ( 0.6854931847115989241, 3.645690833133079956, 8.159427574546592510 ) ) ;
#6223 = CARTESIAN_POINT ( 'NONE',  ( -3.179822820152304885, 2.000074507124384837, 0.5625000000000001110 ) ) ;
#6224 = CARTESIAN_POINT ( 'NONE',  ( 2.537500000000000533, 4.049999999999999822, -0.4312500000000004663 ) ) ;
#6225 = VECTOR ( 'NONE', #7971, 39.37007874015748143 ) ;
#6226 = PLANE ( 'NONE',  #559 ) ;
#6227 = ORIENTED_EDGE ( 'NONE', *, *, #7536, .F. ) ;
#6228 = CARTESIAN_POINT ( 'NONE',  ( -0.6836440906233618442, 4.258440652362253331, 8.282496153036678521 ) ) ;
#6229 = APPROVAL ( #4158, 'UNSPECIFIED' ) ;
#6230 = LINE ( 'NONE', #4918, #3603 ) ;
#6231 = COORDINATED_UNIVERSAL_TIME_OFFSET ( 0, 0, .AHEAD. ) ;
#6232 =( BOUNDED_CURVE ( )  B_SPLINE_CURVE ( 2, ( #2872, #2253, #332, #6031, #5995, #996, #5278 ),
 .UNSPECIFIED., .F., .T. ) 
 B_SPLINE_CURVE_WITH_KNOTS ( ( 3, 2, 2, 3 ),
 ( 2.010031869259635242E-11, 0.003869794796933458212, 0.03119827455188316570, 0.05852675430952081204 ),
 .UNSPECIFIED. ) 
 CURVE ( )  GEOMETRIC_REPRESENTATION_ITEM ( )  RATIONAL_B_SPLINE_CURVE ( ( 0.9287967259844018830, 0.9585254409137464737, 1.000000000000000000, 0.7071067811865479058, 1.000000000000000000, 0.7071067811865479058, 1.000000000000000000 ) ) 
 REPRESENTATION_ITEM ( '' )  );
#6233 = ORIENTED_EDGE ( 'NONE', *, *, #6984, .F. ) ;
#6234 = CARTESIAN_POINT ( 'NONE',  ( -1.500000000000000444, 5.639000000000001123, 0.1249999999999999029 ) ) ;
#6235 = AXIS2_PLACEMENT_3D ( 'NONE', #1136, #4898, #7434 ) ;
#6236 = DIRECTION ( 'NONE',  ( 0.000000000000000000, 0.000000000000000000, 1.000000000000000000 ) ) ;
#6237 = DIRECTION ( 'NONE',  ( 0.000000000000000000, 0.000000000000000000, 1.000000000000000000 ) ) ;
#6238 = EDGE_CURVE ( 'NONE', #6815, #3578, #5162, .T. ) ;
#6239 = VERTEX_POINT ( 'NONE', #6963 ) ;
#6240 = VERTEX_POINT ( 'NONE', #655 ) ;
#6241 = AXIS2_PLACEMENT_3D ( 'NONE', #1302, #4450, #2499 ) ;
#6242 = AXIS2_PLACEMENT_3D ( 'NONE', #6448, #3327, #5241 ) ;
#6243 = CARTESIAN_POINT ( 'NONE',  ( 2.537500000000000533, 1.664000000000000368, 0.000000000000000000 ) ) ;
#6244 = CARTESIAN_POINT ( 'NONE',  ( 0.8148948373165970649, 2.920888456407634060, -5.108749999999998792 ) ) ;
#6245 = PLANE ( 'NONE',  #8116 ) ;
#6246 = ORIENTED_EDGE ( 'NONE', *, *, #5493, .T. ) ;
#6247 = AXIS2_PLACEMENT_3D ( 'NONE', #3730, #3692, #5648 ) ;
#6248 = APPROVAL_STATUS ( 'not_yet_approved' ) ;
#6249 = CARTESIAN_POINT ( 'NONE',  ( -2.740000000000000657, 7.964000000000000412, 3.333750000000001990 ) ) ;
#6250 = CARTESIAN_POINT ( 'NONE',  ( -0.7456179150311872394, 3.868434268270091625, 8.533094314006417491 ) ) ;
#6251 = ORIENTED_EDGE ( 'NONE', *, *, #4125, .F. ) ;
#6252 = ADVANCED_FACE ( 'NONE', ( #6312 ), #693, .F. ) ;
#6253 = ADVANCED_FACE ( 'NONE', ( #3400 ), #2214, .T. ) ;
#6254 = FACE_OUTER_BOUND ( 'NONE', #365, .T. ) ;
#6255 = DIRECTION ( 'NONE',  ( -0.7071067811865474617, 0.000000000000000000, 0.7071067811865474617 ) ) ;
#6256 = CARTESIAN_POINT ( 'NONE',  ( 0.000000000000000000, 3.950000000000000178, -4.308749999765625560 ) ) ;
#6257 = EDGE_LOOP ( 'NONE', ( #5535, #5454, #2482, #2382 ) ) ;
#6258 = PERSON_AND_ORGANIZATION ( #7862, #8117 ) ;
#6259 = CYLINDRICAL_SURFACE ( 'NONE', #6872, 4.805751768934915624 ) ;
#6260 = CONTEXT_DEPENDENT_SHAPE_REPRESENTATION ( #2366, #7060 ) ;
#6261 = CARTESIAN_POINT ( 'NONE',  ( 3.562500000000000444, 1.000000000000000222, 2.612499999999998934 ) ) ;
#6262 = CARTESIAN_POINT ( 'NONE',  ( 0.000000000000000000, 3.950000000000000178, 3.691250000234376660 ) ) ;
#6263 = CARTESIAN_POINT ( 'NONE',  ( -3.987046614173229475, 3.766991497692385948, 8.159690390570178309 ) ) ;
#6264 = FACE_OUTER_BOUND ( 'NONE', #2645, .T. ) ;
#6265 = DIRECTION ( 'NONE',  ( 0.000000000000000000, 1.000000000000000000, 0.000000000000000000 ) ) ;
#6266 = ORIENTED_EDGE ( 'NONE', *, *, #5886, .F. ) ;
#6267 = LINE ( 'NONE', #4542, #7554 ) ;
#6268 = CARTESIAN_POINT ( 'NONE',  ( 3.362500000000000711, 1.750000000000000444, 0.000000000000000000 ) ) ;
#6269 = COORDINATED_UNIVERSAL_TIME_OFFSET ( 0, 0, .AHEAD. ) ;
#6270 = ORIENTED_EDGE ( 'NONE', *, *, #6044, .F. ) ;
#6271 = DIRECTION ( 'NONE',  ( 0.5773502691896258421, -0.5773502691896258421, 0.5773502691896258421 ) ) ;
#6272 = CC_DESIGN_DATE_AND_TIME_ASSIGNMENT ( #43, #3044, ( #4483 ) ) ;
#6273 = DIMENSIONAL_EXPONENTS ( 1.000000000000000000, 0.000000000000000000, 0.000000000000000000, 0.000000000000000000, 0.000000000000000000, 0.000000000000000000, 0.000000000000000000 ) ;
#6274 = CARTESIAN_POINT ( 'NONE',  ( 4.462953385826772035, 3.753500037802128375, 8.231249998505111520 ) ) ;
#6275 = CARTESIAN_POINT ( 'NONE',  ( 4.462953385826773811, 4.225666661560476101, 8.231249998505111520 ) ) ;
#6276 = ADVANCED_FACE ( 'NONE', ( #5897 ), #4701, .T. ) ;
#6277 = ADVANCED_FACE ( 'NONE', ( #4041 ), #7870, .T. ) ;
#6278 = CC_DESIGN_SECURITY_CLASSIFICATION ( #3381, ( #1164 ) ) ;
#6279 = ORIENTED_EDGE ( 'NONE', *, *, #6709, .F. ) ;
#6280 = ORIENTED_EDGE ( 'NONE', *, *, #6896, .T. ) ;
#6281 = EDGE_CURVE ( 'NONE', #1699, #2064, #2161, .T. ) ;
#6282 =( REPRESENTATION_RELATIONSHIP ('NONE','NONE', #3256, #6505 ) REPRESENTATION_RELATIONSHIP_WITH_TRANSFORMATION ( #6104 )SHAPE_REPRESENTATION_RELATIONSHIP( ) );
#6283 = CARTESIAN_POINT ( 'NONE',  ( 2.875000000000000888, -3.820994292482255198E-18, -2.975000000000000977 ) ) ;
#6284 = CARTESIAN_POINT ( 'NONE',  ( 1.270916224172242037, 4.288808537913045171, -5.108750000000001457 ) ) ;
#6285 = EDGE_CURVE ( 'NONE', #615, #1080, #5156, .T. ) ;
#6286 = CARTESIAN_POINT ( 'NONE',  ( 1.187500000000000222, 4.274507914002040998, 6.772132732614807971 ) ) ;
#6287 = ORIENTED_EDGE ( 'NONE', *, *, #5247, .T. ) ;
#6288 = APPROVAL_DATE_TIME ( #1446, #7131 ) ;
#6289 = CARTESIAN_POINT ( 'NONE',  ( -8.751021560936518753E-10, 1.000000000000000222, 5.750408897959578548E-10 ) ) ;
#6290 = DIRECTION ( 'NONE',  ( 1.776356839400250465E-15, 0.000000000000000000, -1.000000000000000000 ) ) ;
#6291 = EDGE_CURVE ( 'NONE', #442, #5098, #857, .T. ) ;
#6292 = ORIENTED_EDGE ( 'NONE', *, *, #5683, .T. ) ;
#6293 = LOCAL_TIME ( 0, 37, 23.00000000000000000, #2864 ) ;
#6294 = EDGE_CURVE ( 'NONE', #6003, #6547, #404, .T. ) ;
#6295 = CYLINDRICAL_SURFACE ( 'NONE', #2948, 2.619834094488189269 ) ;
#6296 = CARTESIAN_POINT ( 'NONE',  ( -2.740000000000001545, 7.964000000000000412, 4.313750000000002416 ) ) ;
#6297 = DIRECTION ( 'NONE',  ( 0.000000000000000000, 0.000000000000000000, -1.000000000000000000 ) ) ;
#6298 = ORIENTED_EDGE ( 'NONE', *, *, #1919, .F. ) ;
#6299 = EDGE_CURVE ( 'NONE', #1844, #5265, #4244, .T. ) ;
#6300 = COORDINATED_UNIVERSAL_TIME_OFFSET ( 0, 0, .AHEAD. ) ;
#6301 = CARTESIAN_POINT ( 'NONE',  ( 3.484120143574221651E-16, 3.001975734461090560E-16, 2.845000000000001528 ) ) ;
#6302 = CARTESIAN_POINT ( 'NONE',  ( -3.562500000000000444, -3.820994442221351629E-18, 2.975000000000000977 ) ) ;
#6303 = COORDINATED_UNIVERSAL_TIME_OFFSET ( 0, 0, .AHEAD. ) ;
#6304 = FACE_OUTER_BOUND ( 'NONE', #3156, .T. ) ;
#6305 = LINE ( 'NONE', #1268, #3448 ) ;
#6306 = CARTESIAN_POINT ( 'NONE',  ( -3.987046614173228143, 3.839697420785793458, 8.068595639695207211 ) ) ;
#6307 = CARTESIAN_POINT ( 'NONE',  ( 1.172489671196043304, 1.000000000000000444, -3.693357952326151494 ) ) ;
#6308 = FACE_OUTER_BOUND ( 'NONE', #7380, .T. ) ;
#6309 = EDGE_LOOP ( 'NONE', ( #2739, #4466, #256, #5094 ) ) ;
#6310 = DIRECTION ( 'NONE',  ( 0.000000000000000000, 0.000000000000000000, 1.000000000000000000 ) ) ;
#6311 =( CONVERSION_BASED_UNIT ( 'INCH', #7574 ) LENGTH_UNIT ( ) NAMED_UNIT ( #4436 ) );
#6312 = FACE_OUTER_BOUND ( 'NONE', #1174, .T. ) ;
#6313 = PERSON_AND_ORGANIZATION_ROLE ( 'creator' ) ;
#6314 = ORIENTED_EDGE ( 'NONE', *, *, #2500, .F. ) ;
#6315 = FACE_OUTER_BOUND ( 'NONE', #7169, .T. ) ;
#6316 = PLANE ( 'NONE',  #1235 ) ;
#6317 = LINE ( 'NONE', #1358, #5305 ) ;
#6318 = PLANE ( 'NONE',  #6485 ) ;
#6319 = DIRECTION ( 'NONE',  ( -1.000000000000000000, -0.000000000000000000, -0.000000000000000000 ) ) ;
#6320 = EDGE_LOOP ( 'NONE', ( #2899, #7993, #2667, #1212 ) ) ;
#6321 = CC_DESIGN_DATE_AND_TIME_ASSIGNMENT ( #2203, #6422, ( #3008 ) ) ;
#6322 = ORIENTED_EDGE ( 'NONE', *, *, #1694, .F. ) ;
#6323 = ADVANCED_FACE ( 'NONE', ( #6019, #5983 ), #322, .T. ) ;
#6324 = CIRCLE ( 'NONE', #4880, 3.874999999025058539 ) ;
#6325 = CARTESIAN_POINT ( 'NONE',  ( 3.987953385826772390, 3.898199183956782221, 8.041502862977342403 ) ) ;
#6326 = CARTESIAN_POINT ( 'NONE',  ( 1.267418545190977852, 3.608279822688814420, -5.108750000000002345 ) ) ;
#6327 = CARTESIAN_POINT ( 'NONE',  ( 3.987953385826772390, 3.950000015938371689, 8.231249998505111520 ) ) ;
#6328 = ORIENTED_EDGE ( 'NONE', *, *, #1327, .F. ) ;
#6329 = LINE ( 'NONE', #3817, #1916 ) ;
#6330 = EDGE_LOOP ( 'NONE', ( #7718, #7943, #1636, #566, #1067, #4548 ) ) ;
#6331 = VECTOR ( 'NONE', #471, 39.37007874015748143 ) ;
#6332 = CC_DESIGN_APPROVAL ( #3215, ( #2668 ) ) ;
#6333 = LOCAL_TIME ( 0, 37, 23.00000000000000000, #2498 ) ;
#6334 = ADVANCED_FACE ( 'NONE', ( #2126 ), #2742, .T. ) ;
#6335 = VECTOR ( 'NONE', #625, 39.37007874015748143 ) ;
#6336 = DIRECTION ( 'NONE',  ( 0.000000000000000000, 0.000000000000000000, 1.000000000000000000 ) ) ;
#6337 = CARTESIAN_POINT ( 'NONE',  ( 4.462953385826772035, 4.146499994074615003, 8.231249998505111520 ) ) ;
#6338 = ORIENTED_EDGE ( 'NONE', *, *, #1489, .F. ) ;
#6339 = DATE_AND_TIME ( #6794, #5004 ) ;
#6340 = EDGE_CURVE ( 'NONE', #1666, #6815, #7313, .T. ) ;
#6341 = PLANE ( 'NONE',  #463 ) ;
#6342 = SECURITY_CLASSIFICATION_LEVEL ( 'unclassified' ) ;
#6343 = CARTESIAN_POINT ( 'NONE',  ( 2.750000000000002665, 7.339000000000001300, 3.161250000000001670 ) ) ;
#6344 = CIRCLE ( 'NONE', #2151, 1.074999999999999289 ) ;
#6345 = VECTOR ( 'NONE', #748, 39.37007874015748143 ) ;
#6346 = ORIENTED_EDGE ( 'NONE', *, *, #8102, .F. ) ;
#6347 = CARTESIAN_POINT ( 'NONE',  ( 2.740000000000000657, 7.964000000000000412, 3.813750000000002416 ) ) ;
#6348 = CARTESIAN_POINT ( 'NONE',  ( 2.126102704337182736, 1.000000000000000444, -3.279369616689862710 ) ) ;
#6349 = AXIS2_PLACEMENT_3D ( 'NONE', #2778, #3437, #4618 ) ;
#6350 = DIRECTION ( 'NONE',  ( -1.000000000000000000, 0.000000000000000000, 0.000000000000000000 ) ) ;
#6351 = ORIENTED_EDGE ( 'NONE', *, *, #7186, .T. ) ;
#6352 = CARTESIAN_POINT ( 'NONE',  ( 0.000000000000000000, 8.574153543307087233, 4.323750000000000426 ) ) ;
#6353 = CLOSED_SHELL ( 'NONE', ( #6908, #2110, #590, #699, #6756, #6850, #1858, #5616, #1784, #2629, #6428, #5450, #5044, #3031, #7298, #1729, #526, #6136, #1454, #2590, #226, #7589, #2646, #4575, #5524, #3637 ) ) ;
#6354 = SHAPE_REPRESENTATION_RELATIONSHIP ( 'NONE' , 'NONE' ,  #6925, #5458 ) ;
#6355 = CARTESIAN_POINT ( 'NONE',  ( -1.187500000000000444, 4.384350929501749761, 6.623573783009716109 ) ) ;
#6356 = CARTESIAN_POINT ( 'NONE',  ( 0.000000000000000000, 2.500000000000000000, -2.750000000000000444 ) ) ;
#6357 = APPROVAL_STATUS ( 'not_yet_approved' ) ;
#6358 = ORIENTED_EDGE ( 'NONE', *, *, #7384, .F. ) ;
#6359 = PLANE ( 'NONE',  #227 ) ;
#6360 = EDGE_CURVE ( 'NONE', #2985, #7102, #1679, .T. ) ;
#6361 = AXIS2_PLACEMENT_3D ( 'NONE', #617, #7869, #1101 ) ;
#6362 = DIRECTION ( 'NONE',  ( -0.000000000000000000, -0.000000000000000000, 1.000000000000000000 ) ) ;
#6363 = FACE_OUTER_BOUND ( 'NONE', #31, .T. ) ;
#6364 = ORIENTED_EDGE ( 'NONE', *, *, #2784, .F. ) ;
#6365 = VERTEX_POINT ( 'NONE', #989 ) ;
#6366 = CIRCLE ( 'NONE', #2833, 1.249999999999999556 ) ;
#6367 = VECTOR ( 'NONE', #401, 39.37007874015748143 ) ;
#6368 = CARTESIAN_POINT ( 'NONE',  ( 3.987953385826774166, 3.887887077482501397, 8.044773094730341967 ) ) ;
#6369 = CARTESIAN_POINT ( 'NONE',  ( 1.196592964269871384, 4.489712393535192803, -5.108750000000001457 ) ) ;
#6370 = DIRECTION ( 'NONE',  ( 1.000000000000000000, 0.000000000000000000, 0.000000000000000000 ) ) ;
#6371 = CARTESIAN_POINT ( 'NONE',  ( 3.987953385826772390, 3.773847781579248828, 8.318774035908578668 ) ) ;
#6372 = CARTESIAN_POINT ( 'NONE',  ( 0.000000000000000000, 5.137500000000000178, 6.956250000000000711 ) ) ;
#6373 = AXIS2_PLACEMENT_3D ( 'NONE', #2977, #4361, #2458 ) ;
#6374 = ORIENTED_EDGE ( 'NONE', *, *, #3639, .T. ) ;
#6375 = VECTOR ( 'NONE', #8072, 39.37007874015748143 ) ;
#6376 = APPROVAL ( #1055, 'UNSPECIFIED' ) ;
#6377 = VECTOR ( 'NONE', #7014, 39.37007874015748143 ) ;
#6378 = DIRECTION ( 'NONE',  ( 0.000000000000000000, 0.000000000000000000, -1.000000000000000000 ) ) ;
#6379 = CARTESIAN_POINT ( 'NONE',  ( 3.182000000000000828, 5.541000000000003922, 3.956250000000000266 ) ) ;
#6380 = VERTEX_POINT ( 'NONE', #3485 ) ;
#6381 = PERSON_AND_ORGANIZATION_ROLE ( 'classification_officer' ) ;
#6382 = FACE_OUTER_BOUND ( 'NONE', #4696, .T. ) ;
#6383 = APPROVAL_DATE_TIME ( #4532, #2066 ) ;
#6384 = DIRECTION ( 'NONE',  ( -2.664535259084986204E-15, 0.000000000000000000, 1.000000000000000000 ) ) ;
#6385 = CARTESIAN_POINT ( 'NONE',  ( -1.347488132453362963, 2.365290551065806213, -2.750000000000000444 ) ) ;
#6386 = DIRECTION ( 'NONE',  ( -0.000000000000000000, 1.000000000000000000, 0.000000000000000000 ) ) ;
#6387 = VERTEX_POINT ( 'NONE', #1638 ) ;
#6388 = DIRECTION ( 'NONE',  ( -0.000000000000000000, -1.000000000000000000, -0.000000000000000000 ) ) ;
#6389 = CARTESIAN_POINT ( 'NONE',  ( 2.724999998660272205, 3.550000000000001155, 2.790532913385826763 ) ) ;
#6390 = CARTESIAN_POINT ( 'NONE',  ( -3.987046614173229919, 4.033008582717316770, 8.409411560744450398 ) ) ;
#6391 = ORIENTED_EDGE ( 'NONE', *, *, #3383, .F. ) ;
#6392 = CARTESIAN_POINT ( 'NONE',  ( -3.987046614173228587, 4.146499994074616779, 8.231249998505111520 ) ) ;
#6393 = CARTESIAN_POINT ( 'NONE',  ( -1.187500000000000666, 4.766349921454176020, 5.658050103701500078 ) ) ;
#6394 = CARTESIAN_POINT ( 'NONE',  ( 1.624999999999999778, 3.950000000000000178, -5.108750000000001457 ) ) ;
#6395 = COORDINATED_UNIVERSAL_TIME_OFFSET ( 0, 0, .AHEAD. ) ;
#6396 = APPROVAL_PERSON_ORGANIZATION ( #3803, #5165, #5117 ) ;
#6397 = ORIENTED_EDGE ( 'NONE', *, *, #3027, .F. ) ;
#6398 = EDGE_CURVE ( 'NONE', #5712, #6928, #362, .T. ) ;
#6399 =( REPRESENTATION_RELATIONSHIP ('NONE','NONE', #3256, #7355 ) REPRESENTATION_RELATIONSHIP_WITH_TRANSFORMATION ( #2247 )SHAPE_REPRESENTATION_RELATIONSHIP( ) );
#6400 = CC_DESIGN_APPROVAL ( #7709, ( #1164 ) ) ;
#6401 = CARTESIAN_POINT ( 'NONE',  ( 0.000000000000000000, 3.950000000000000178, -5.108750000000001457 ) ) ;
#6402 =( NAMED_UNIT ( * ) PLANE_ANGLE_UNIT ( ) SI_UNIT ( $, .RADIAN. ) );
#6403 = DIRECTION ( 'NONE',  ( -1.000000000000000000, -0.000000000000000000, -0.000000000000000000 ) ) ;
#6404 = ADVANCED_FACE ( 'NONE', ( #2863 ), #7176, .F. ) ;
#6405 = EDGE_CURVE ( 'NONE', #2476, #2954, #2287, .T. ) ;
#6406 = ORIENTED_EDGE ( 'NONE', *, *, #317, .T. ) ;
#6407 = PLANE ( 'NONE',  #2972 ) ;
#6408 = CARTESIAN_POINT ( 'NONE',  ( 0.7077600209949285182, 3.701565529548708433, 8.421896151506288675 ) ) ;
#6409 = ORIENTED_EDGE ( 'NONE', *, *, #2686, .F. ) ;
#6410 = CARTESIAN_POINT ( 'NONE',  ( 3.987953385826772390, 3.761880377346017656, 8.173848920211581159 ) ) ;
#6411 = CARTESIAN_POINT ( 'NONE',  ( 0.04453716361813374325, 5.262460292302547415, -5.108750000000001457 ) ) ;
#6412 = DIRECTION ( 'NONE',  ( 0.000000000000000000, 0.000000000000000000, 1.000000000000000000 ) ) ;
#6413 = EDGE_CURVE ( 'NONE', #4886, #1701, #4785, .T. ) ;
#6414 = CARTESIAN_POINT ( 'NONE',  ( -2.750000000000000444, 8.719000000000001194, 3.813750000000002416 ) ) ;
#6415 = ORIENTED_EDGE ( 'NONE', *, *, #5367, .T. ) ;
#6416 = CARTESIAN_POINT ( 'NONE',  ( -2.750000000000000444, 8.719000000000002970, 4.313750000000002416 ) ) ;
#6417 = DIRECTION ( 'NONE',  ( 0.000000000000000000, 0.000000000000000000, 1.000000000000000000 ) ) ;
#6418 = ORIENTED_EDGE ( 'NONE', *, *, #3383, .T. ) ;
#6419 = LOCAL_TIME ( 0, 37, 23.00000000000000000, #4909 ) ;
#6420 = CALENDAR_DATE ( 2026, 8, 10 ) ;
#6421 = PLANE ( 'NONE',  #2437 ) ;
#6422 = DATE_TIME_ROLE ( 'classification_date' ) ;
#6423 = CARTESIAN_POINT ( 'NONE',  ( 3.562500000000000444, -0.000000000000000000, 2.975000000000000977 ) ) ;
#6424 = PRODUCT_DEFINITION ( 'UNKNOWN', '', #8153, #7792 ) ;
#6425 = DIRECTION ( 'NONE',  ( -3.552713678812811104E-15, 0.000000000000000000, 1.000000000000000000 ) ) ;
#6426 = LINE ( 'NONE', #804, #6512 ) ;
#6427 = ORIENTED_EDGE ( 'NONE', *, *, #4079, .F. ) ;
#6428 = ADVANCED_FACE ( 'NONE', ( #2375 ), #6760, .F. ) ;
#6429 = CARTESIAN_POINT ( 'NONE',  ( -3.987046614173228143, 4.021559623873138811, 8.048241480259026304 ) ) ;
#6430 = LINE ( 'NONE', #143, #7447 ) ;
#6431 = CARTESIAN_POINT ( 'NONE',  ( -3.987046614173229475, 4.139745409976819168, 8.283055230728985308 ) ) ;
#6432 = ORIENTED_EDGE ( 'NONE', *, *, #7681, .F. ) ;
#6433 = DIRECTION ( 'NONE',  ( -0.000000000000000000, 1.000000000000000000, 0.000000000000000000 ) ) ;
#6434 = ORIENTED_EDGE ( 'NONE', *, *, #1662, .F. ) ;
#6435 = DIRECTION ( 'NONE',  ( 0.0005594472316433852718, -3.267255455926554204E-16, 0.9999998435093852001 ) ) ;
#6436 = CARTESIAN_POINT ( 'NONE',  ( 2.750000000000000444, 7.339000000000003077, 5.236250000000000071 ) ) ;
#6437 = CARTESIAN_POINT ( 'NONE',  ( 2.750000000000000444, 7.973999999999999311, 3.833750000000001545 ) ) ;
#6438 = APPROVAL_DATE_TIME ( #324, #4358 ) ;
#6439 = VERTEX_POINT ( 'NONE', #7441 ) ;
#6440 = ADVANCED_FACE ( 'NONE', ( #1801 ), #2939, .T. ) ;
#6441 = DIRECTION ( 'NONE',  ( -0.000000000000000000, -0.000000000000000000, 1.000000000000000000 ) ) ;
#6442 =( LENGTH_UNIT ( ) NAMED_UNIT ( * ) SI_UNIT ( $, .METRE. ) );
#6443 = CARTESIAN_POINT ( 'NONE',  ( 2.875000000000000888, 1.000000000000000222, -2.975000000000000977 ) ) ;
#6444 = PERSON_AND_ORGANIZATION ( #7862, #8117 ) ;
#6445 =( REPRESENTATION_RELATIONSHIP ('NONE','NONE', #3256, #4229 ) REPRESENTATION_RELATIONSHIP_WITH_TRANSFORMATION ( #4161 )SHAPE_REPRESENTATION_RELATIONSHIP( ) );
#6446 = ORIENTED_EDGE ( 'NONE', *, *, #849, .T. ) ;
#6447 = EDGE_CURVE ( 'NONE', #5577, #1477, #4944, .T. ) ;
#6448 = CARTESIAN_POINT ( 'NONE',  ( -8.751021560936518753E-10, 1.000000000000000222, 5.750408897959578548E-10 ) ) ;
#6449 = ORIENTED_EDGE ( 'NONE', *, *, #2917, .F. ) ;
#6450 = UNCERTAINTY_MEASURE_WITH_UNIT (LENGTH_MEASURE( 1.000000000000000082E-05 ), #7737, 'distance_accuracy_value', 'NONE');
#6451 =( BOUNDED_CURVE ( )  B_SPLINE_CURVE ( 3, ( #4771, #3006, #5546, #4148 ),
 .UNSPECIFIED., .F., .F. ) 
 B_SPLINE_CURVE_WITH_KNOTS ( ( 4, 4 ),
 ( 1.016459758734699301E-17, 0.2669680800879517535 ),
 .UNSPECIFIED. ) 
 CURVE ( )  GEOMETRIC_REPRESENTATION_ITEM ( )  RATIONAL_B_SPLINE_CURVE ( ( 1.000000000000000000, 0.3333333333333334259, 0.3333333333333334259, 1.000000000000000000 ) ) 
 REPRESENTATION_ITEM ( '' )  );
#6452 = EDGE_CURVE ( 'NONE', #4681, #8092, #1835, .T. ) ;
#6453 = CARTESIAN_POINT ( 'NONE',  ( 3.987953385826772390, 3.787345657128307508, 8.120947403352559490 ) ) ;
#6454 = AXIS2_PLACEMENT_3D ( 'NONE', #5593, #6985, #7555 ) ;
#6455 = CARTESIAN_POINT ( 'NONE',  ( -2.740000000000001545, 8.729000000000002757, 3.833750000000001545 ) ) ;
#6456 = PLANE ( 'NONE',  #1262 ) ;
#6457 = CARTESIAN_POINT ( 'NONE',  ( 3.987953385826773278, 4.146499994074616779, 8.243275897752392112 ) ) ;
#6458 = VERTEX_POINT ( 'NONE', #6830 ) ;
#6459 = AXIS2_PLACEMENT_3D ( 'NONE', #318, #1167, #4932 ) ;
#6460 = VECTOR ( 'NONE', #4063, 39.37007874015748143 ) ;
#6461 = LOCAL_TIME ( 0, 37, 23.00000000000000000, #3937 ) ;
#6462 = CARTESIAN_POINT ( 'NONE',  ( -2.750000000000000444, 7.964000000000000412, 3.323750000000001759 ) ) ;
#6463 = DIRECTION ( 'NONE',  ( -1.000000000000000000, 0.000000000000000000, 0.000000000000000000 ) ) ;
#6464 = AXIS2_PLACEMENT_3D ( 'NONE', #1997, #896, #5732 ) ;
#6465 = EDGE_LOOP ( 'NONE', ( #5431, #6322, #5960 ) ) ;
#6466 = APPROVAL_ROLE ( '' ) ;
#6467 = AXIS2_PLACEMENT_3D ( 'NONE', #6190, #7280, #6660 ) ;
#6468 = CARTESIAN_POINT ( 'NONE',  ( 1.312500000000000444, 4.908106850393701315, 3.316250000000001474 ) ) ;
#6469 = APPROVAL_PERSON_ORGANIZATION ( #7835, #3007, #3446 ) ;
#6470 = CALENDAR_DATE ( 2026, 8, 10 ) ;
#6471 = CARTESIAN_POINT ( 'NONE',  ( 2.750000000000000444, 7.964000000000000412, 4.313750000000002416 ) ) ;
#6472 = CARTESIAN_POINT ( 'NONE',  ( 4.462953385826772035, 3.753500037802128375, 8.231249998505111520 ) ) ;
#6473 = DIRECTION ( 'NONE',  ( -0.000000000000000000, 1.000000000000000000, 0.000000000000000000 ) ) ;
#6474 = PRODUCT_DEFINITION_SHAPE ( 'NONE', 'NONE',  #6586 ) ;
#6475 = VECTOR ( 'NONE', #6891, 39.37007874015748854 ) ;
#6476 = ORIENTED_EDGE ( 'NONE', *, *, #2882, .F. ) ;
#6477 = CARTESIAN_POINT ( 'NONE',  ( -3.987046614173229475, 3.919106724554535681, 8.426027723965566096 ) ) ;
#6478 = ORIENTED_EDGE ( 'NONE', *, *, #2383, .F. ) ;
#6479 = CARTESIAN_POINT ( 'NONE',  ( 0.000000000000000000, 5.541000000000003034, 3.956250000000000266 ) ) ;
#6480 = CARTESIAN_POINT ( 'NONE',  ( -2.001218421989477747, 8.759198453399624995, 8.676429074610400249 ) ) ;
#6481 = CARTESIAN_POINT ( 'NONE',  ( -8.751021560936518753E-10, 1.365923996832131609E-16, 3.874999999600099443 ) ) ;
#6482 = DATE_AND_TIME ( #2825, #6918 ) ;
#6483 = EDGE_LOOP ( 'NONE', ( #3495, #1384, #577, #3403 ) ) ;
#6484 = AXIS2_PLACEMENT_3D ( 'NONE', #1608, #995, #3491 ) ;
#6485 = AXIS2_PLACEMENT_3D ( 'NONE', #7279, #3848, #663 ) ;
#6486 = VECTOR ( 'NONE', #6530, 39.37007874015748143 ) ;
#6487 = DIRECTION ( 'NONE',  ( 0.000000000000000000, -1.000000000000000000, 0.000000000000000000 ) ) ;
#6488 = AXIS2_PLACEMENT_3D ( 'NONE', #7854, #2154, #2200 ) ;
#6489 = APPROVAL ( #7205, 'UNSPECIFIED' ) ;
#6490 = DIRECTION ( 'NONE',  ( 0.3026345437601030697, 0.000000000000000000, 0.9531066744720204653 ) ) ;
#6491 = CARTESIAN_POINT ( 'NONE',  ( 2.750000000000000444, 7.339000000000001300, 3.161250000000001670 ) ) ;
#6492 = DIRECTION ( 'NONE',  ( -0.000000000000000000, -0.000000000000000000, 1.000000000000000000 ) ) ;
#6493 = ORIENTED_EDGE ( 'NONE', *, *, #2305, .F. ) ;
#6494 = COORDINATED_UNIVERSAL_TIME_OFFSET ( 0, 0, .AHEAD. ) ;
#6495 = ORIENTED_EDGE ( 'NONE', *, *, #4589, .T. ) ;
#6496 = LINE ( 'NONE', #3368, #1543 ) ;
#6497 = EDGE_CURVE ( 'NONE', #5577, #5222, #3056, .T. ) ;
#6498 = EDGE_CURVE ( 'NONE', #5226, #2362, #7521, .T. ) ;
#6499 = VECTOR ( 'NONE', #1628, 39.37007874015748143 ) ;
#6500 = LINE ( 'NONE', #874, #4091 ) ;
#6501 = CARTESIAN_POINT ( 'NONE',  ( -2.740000000000000213, 8.729000000000002757, 3.813750000000002416 ) ) ;
#6502 = CARTESIAN_POINT ( 'NONE',  ( -3.562500000000000444, 0.000000000000000000, 3.337500000000003020 ) ) ;
#6503 = ORIENTED_EDGE ( 'NONE', *, *, #6360, .T. ) ;
#6504 = CARTESIAN_POINT ( 'NONE',  ( 3.987953385826772390, 4.028498573891106105, 8.411512280006094855 ) ) ;
#6505 = SHAPE_REPRESENTATION ( 'bench vise2-', ( #7272 ), #2811 ) ;
#6506 = ORIENTED_EDGE ( 'NONE', *, *, #2933, .T. ) ;
#6507 = AXIS2_PLACEMENT_3D ( 'NONE', #3275, #151, #7056 ) ;
#6508 = VECTOR ( 'NONE', #344, 39.37007874015748143 ) ;
#6509 = DIRECTION ( 'NONE',  ( -0.3026345437736693289, -0.000000000000000000, 0.9531066744677130220 ) ) ;
#6510 = DIRECTION ( 'NONE',  ( 0.000000000000000000, 1.000000000000000000, 0.000000000000000000 ) ) ;
#6511 = LINE ( 'NONE', #307, #7137 ) ;
#6512 = VECTOR ( 'NONE', #5806, 39.37007874015748143 ) ;
#6513 = ORIENTED_EDGE ( 'NONE', *, *, #548, .F. ) ;
#6514 = MECHANICAL_CONTEXT ( 'NONE', #3147, 'mechanical' ) ;
#6515 = APPLICATION_CONTEXT ( 'configuration controlled 3d designs of mechanical parts and assemblies' ) ;
#6516 = CARTESIAN_POINT ( 'NONE',  ( -0.7499999999999993339, 3.950000000000000178, 8.543750000000002842 ) ) ;
#6517 = EDGE_CURVE ( 'NONE', #1993, #7244, #7276, .T. ) ;
#6518 = DATE_AND_TIME ( #7123, #2802 ) ;
#6519 = CARTESIAN_POINT ( 'NONE',  ( -1.624999999999999112, 3.950000000000000178, 2.749999999206901968 ) ) ;
#6520 = EDGE_CURVE ( 'NONE', #2223, #1240, #6103, .T. ) ;
#6521 = CARTESIAN_POINT ( 'NONE',  ( -1.624999999336056877, 2.076218724820237060, -2.750000000000000444 ) ) ;
#6522 = CARTESIAN_POINT ( 'NONE',  ( -1.312500000000000444, 4.908106850393701315, 0.5414159055118122899 ) ) ;
#6523 = AXIS2_PLACEMENT_3D ( 'NONE', #5344, #7901, #2 ) ;
#6524 = VECTOR ( 'NONE', #89, 39.37007874015748143 ) ;
#6525 = ORIENTED_EDGE ( 'NONE', *, *, #2500, .T. ) ;
#6526 = CARTESIAN_POINT ( 'NONE',  ( -3.987046614173229919, 3.769836505190808928, 8.309711754443199538 ) ) ;
#6527 = CARTESIAN_POINT ( 'NONE',  ( -1.312500000000000444, 5.414000000000000590, 3.316250000000001474 ) ) ;
#6528 = CARTESIAN_POINT ( 'NONE',  ( 0.7499999999999993339, 3.950000000000000178, 7.918749999999998401 ) ) ;
#6529 = EDGE_LOOP ( 'NONE', ( #1331, #4614, #1024, #2890, #952, #7695, #4521, #5581 ) ) ;
#6530 = DIRECTION ( 'NONE',  ( 0.000000000000000000, 0.000000000000000000, 1.000000000000000000 ) ) ;
#6531 = LINE ( 'NONE', #2709, #1658 ) ;
#6532 = PERSON_AND_ORGANIZATION_ROLE ( 'classification_officer' ) ;
#6533 = AXIS2_PLACEMENT_3D ( 'NONE', #2589, #2550, #6887 ) ;
#6534 = EDGE_LOOP ( 'NONE', ( #597, #7310, #4351, #3559 ) ) ;
#6535 = CARTESIAN_POINT ( 'NONE',  ( -1.312363187401233144, 4.037659949503647816, -5.108749999999999680 ) ) ;
#6536 = DIRECTION ( 'NONE',  ( 0.000000000000000000, -1.000000000000000000, -0.000000000000000000 ) ) ;
#6537 = APPROVAL_PERSON_ORGANIZATION ( #739, #98, #5036 ) ;
#6538 = CARTESIAN_POINT ( 'NONE',  ( 2.537499998660271761, 3.550000000000001155, 0.3883559095726498156 ) ) ;
#6539 = EDGE_LOOP ( 'NONE', ( #6869, #3482 ) ) ;
#6540 = PERSON_AND_ORGANIZATION_ROLE ( 'design_owner' ) ;
#6541 = EDGE_LOOP ( 'NONE', ( #3107, #3580, #1347, #5662 ) ) ;
#6542 = CARTESIAN_POINT ( 'NONE',  ( -0.7499999999999993339, 3.950000000000000178, 7.918749999999998401 ) ) ;
#6543 = CARTESIAN_POINT ( 'NONE',  ( 0.7314405957411594938, 3.783958348137105965, 8.496183445665874245 ) ) ;
#6544 = APPROVAL ( #2716, 'UNSPECIFIED' ) ;
#6545 = DIRECTION ( 'NONE',  ( -0.000000000000000000, -1.000000000000000000, -0.000000000000000000 ) ) ;
#6546 = CARTESIAN_POINT ( 'NONE',  ( 4.462953385826771147, 4.146499994074616779, 7.838250042232624892 ) ) ;
#6547 = VERTEX_POINT ( 'NONE', #444 ) ;
#6548 = CARTESIAN_POINT ( 'NONE',  ( 3.987953385826772390, 4.100522301782647538, 8.357885377187420417 ) ) ;
#6549 = CARTESIAN_POINT ( 'NONE',  ( -0.7188803599037372205, 3.736068989823152275, 8.459265585397702125 ) ) ;
#6550 = ORIENTED_EDGE ( 'NONE', *, *, #1173, .F. ) ;
#6551 = EDGE_CURVE ( 'NONE', #5487, #3887, #4291, .T. ) ;
#6552 = CARTESIAN_POINT ( 'NONE',  ( 0.000000000000000000, 1.750000000000000666, 0.000000000000000000 ) ) ;
#6553 = EDGE_CURVE ( 'NONE', #5810, #4517, #7015, .T. ) ;
#6554 = LINE ( 'NONE', #6667, #6508 ) ;
#6555 = ADVANCED_FACE ( 'NONE', ( #1179 ), #3680, .T. ) ;
#6556 = CARTESIAN_POINT ( 'NONE',  ( 0.000000000000000000, 5.639000000000001123, -2.750000000000000444 ) ) ;
#6557 = CARTESIAN_POINT ( 'NONE',  ( 0.000000000000000000, 8.719000000000002970, 4.323750000000001315 ) ) ;
#6558 = MECHANICAL_CONTEXT ( 'NONE', #905, 'mechanical' ) ;
#6559 = PLANE ( 'NONE',  #3092 ) ;
#6560 = CONTEXT_DEPENDENT_SHAPE_REPRESENTATION ( #525, #1837 ) ;
#6561 = CARTESIAN_POINT ( 'NONE',  ( 0.7253671533374044245, 3.759190173666904222, 7.983559312723938817 ) ) ;
#6562 = LINE ( 'NONE', #5220, #6111 ) ;
#6563 = ADVANCED_FACE ( 'NONE', ( #8036 ), #7071, .T. ) ;
#6564 = ORIENTED_EDGE ( 'NONE', *, *, #228, .T. ) ;
#6565 =( REPRESENTATION_RELATIONSHIP ('NONE','NONE', #3570, #6040 ) REPRESENTATION_RELATIONSHIP_WITH_TRANSFORMATION ( #3300 )SHAPE_REPRESENTATION_RELATIONSHIP( ) );
#6566 = PLANE ( 'NONE',  #342 ) ;
#6567 = CARTESIAN_POINT ( 'NONE',  ( -3.987046614173229475, 4.121369605927847957, 8.327459834506157677 ) ) ;
#6568 = VERTEX_POINT ( 'NONE', #3791 ) ;
#6569 = CARTESIAN_POINT ( 'NONE',  ( -3.182000000000000828, 2.359000000000000874, 3.956250000000000266 ) ) ;
#6570 = ORIENTED_EDGE ( 'NONE', *, *, #7951, .F. ) ;
#6571 =( NAMED_UNIT ( * ) SI_UNIT ( $, .STERADIAN. ) SOLID_ANGLE_UNIT ( ) );
#6572 = CARTESIAN_POINT ( 'NONE',  ( -1.201750196850394081, 2.500000000000000444, -2.750000000000000444 ) ) ;
#6573 = PERSON_AND_ORGANIZATION_ROLE ( 'creator' ) ;
#6574 = ORIENTED_EDGE ( 'NONE', *, *, #3130, .F. ) ;
#6575 = ADVANCED_FACE ( 'NONE', ( #3827 ), #5101, .T. ) ;
#6576 = PRODUCT_DEFINITION_FORMATION_WITH_SPECIFIED_SOURCE ( 'ANY', '', #4489, .NOT_KNOWN. ) ;
#6577 = FACE_OUTER_BOUND ( 'NONE', #6793, .T. ) ;
#6578 = CARTESIAN_POINT ( 'NONE',  ( -1.301660623695976904, 3.780290714801028962, -5.108749999999998792 ) ) ;
#6579 = ADVANCED_FACE ( 'NONE', ( #1425 ), #6421, .T. ) ;
#6580 = LINE ( 'NONE', #2787, #5671 ) ;
#6581 = DIRECTION ( 'NONE',  ( 0.000000000000000000, -0.7071067811865475727, -0.7071067811865475727 ) ) ;
#6582 = DATE_AND_TIME ( #950, #532 ) ;
#6583 = EDGE_LOOP ( 'NONE', ( #5142, #7861, #3090, #321, #5307, #3116, #3818, #7690 ) ) ;
#6584 = FACE_OUTER_BOUND ( 'NONE', #4181, .T. ) ;
#6585 = DIRECTION ( 'NONE',  ( 0.000000000000000000, 0.000000000000000000, 1.000000000000000000 ) ) ;
#6586 = PRODUCT_DEFINITION ( 'UNKNOWN', '', #1164, #1368 ) ;
#6587 = LINE ( 'NONE', #2842, #163 ) ;
#6588 = CARTESIAN_POINT ( 'NONE',  ( 3.987953385826772390, 3.872296061808989442, 8.411747167338544884 ) ) ;
#6589 = CARTESIAN_POINT ( 'NONE',  ( -0.7078558382242211566, 3.701833123853966345, 8.422262045139364162 ) ) ;
#6590 = EDGE_LOOP ( 'NONE', ( #7198, #5051 ) ) ;
#6591 = CARTESIAN_POINT ( 'NONE',  ( -3.987046614173228143, 4.028498573889014445, 8.050987717002875854 ) ) ;
#6592 = DIRECTION ( 'NONE',  ( 0.000000000000000000, 0.000000000000000000, -1.000000000000000000 ) ) ;
#6593 = CC_DESIGN_PERSON_AND_ORGANIZATION_ASSIGNMENT ( #7563, #4408, ( #7249 ) ) ;
#6594 = LINE ( 'NONE', #5337, #7559 ) ;
#6595 = ORIENTED_EDGE ( 'NONE', *, *, #5586, .F. ) ;
#6596 = APPROVAL_DATE_TIME ( #4066, #6489 ) ;
#6597 = LINE ( 'NONE', #1591, #5292 ) ;
#6598 = DIRECTION ( 'NONE',  ( -0.7071067811865475727, -0.000000000000000000, 0.7071067811865475727 ) ) ;
#6599 = CC_DESIGN_APPROVAL ( #7614, ( #2137 ) ) ;
#6600 = CARTESIAN_POINT ( 'NONE',  ( 0.000000000000000000, 5.538300220770111082, 4.041069104531357148 ) ) ;
#6601 = EDGE_CURVE ( 'NONE', #5813, #3411, #2295, .T. ) ;
#6602 = ORIENTED_EDGE ( 'NONE', *, *, #3104, .T. ) ;
#6603 = FACE_OUTER_BOUND ( 'NONE', #2596, .T. ) ;
#6604 = AXIS2_PLACEMENT_3D ( 'NONE', #6074, #2350, #7366 ) ;
#6605 = ADVANCED_FACE ( 'NONE', ( #7683 ), #6341, .T. ) ;
#6606 = LOCAL_TIME ( 0, 37, 23.00000000000000000, #7896 ) ;
#6607 = CARTESIAN_POINT ( 'NONE',  ( 3.343750000000001776, 1.750000000000000444, 3.383875000000000632 ) ) ;
#6608 = CARTESIAN_POINT ( 'NONE',  ( 0.000000000000000000, 2.359000000000000874, 3.956250000000000266 ) ) ;
#6609 = CARTESIAN_POINT ( 'NONE',  ( 2.537500000000000533, 2.500000000000000444, 0.000000000000000000 ) ) ;
#6610 = ORIENTED_EDGE ( 'NONE', *, *, #7364, .F. ) ;
#6611 = MECHANICAL_CONTEXT ( 'NONE', #2730, 'mechanical' ) ;
#6612 =( BOUNDED_CURVE ( )  B_SPLINE_CURVE ( 3, ( #5630, #4322, #1209, #1750 ),
 .UNSPECIFIED., .F., .F. ) 
 B_SPLINE_CURVE_WITH_KNOTS ( ( 4, 4 ),
 ( 0.000000000000000000, 0.03375796090494045942 ),
 .UNSPECIFIED. ) 
 CURVE ( )  GEOMETRIC_REPRESENTATION_ITEM ( )  RATIONAL_B_SPLINE_CURVE ( ( 0.9995642358097424074, 0.7927633097668024265, 0.6501402846732283747, 0.5716951605290202520 ) ) 
 REPRESENTATION_ITEM ( '' )  );
#6613 = CARTESIAN_POINT ( 'NONE',  ( -2.750000000000000444, 8.729000000000002757, 3.813750000000002416 ) ) ;
#6614 = MECHANICAL_CONTEXT ( 'NONE', #5547, 'mechanical' ) ;
#6615 = ORIENTED_EDGE ( 'NONE', *, *, #5095, .T. ) ;
#6616 = CARTESIAN_POINT ( 'NONE',  ( 1.312500000123273169, 7.352492868468935683, 3.316250000424603606 ) ) ;
#6617 = VECTOR ( 'NONE', #7607, 39.37007874015748854 ) ;
#6618 = CARTESIAN_POINT ( 'NONE',  ( -1.242854508572050598, 4.374042214390413186, -5.108749999999998792 ) ) ;
#6619 = DIRECTION ( 'NONE',  ( 0.000000000000000000, 0.000000000000000000, -1.000000000000000000 ) ) ;
#6620 = AXIS2_PLACEMENT_3D ( 'NONE', #8055, #2390, #3734 ) ;
#6621 = CARTESIAN_POINT ( 'NONE',  ( 3.583510604133040900, 1.543025754838327046, 0.000000000000000000 ) ) ;
#6622 = APPROVAL_DATE_TIME ( #210, #6544 ) ;
#6623 = VERTEX_POINT ( 'NONE', #800 ) ;
#6624 = LINE ( 'NONE', #7275, #6899 ) ;
#6625 = UNCERTAINTY_MEASURE_WITH_UNIT (LENGTH_MEASURE( 1.000000000000000082E-05 ), #4700, 'distance_accuracy_value', 'NONE');
#6626 = VECTOR ( 'NONE', #347, 39.37007874015748143 ) ;
#6627 = CARTESIAN_POINT ( 'NONE',  ( 0.5199956572608818162, 5.160877715126503951, 6.858307716535437137 ) ) ;
#6628 = AXIS2_PLACEMENT_3D ( 'NONE', #3753, #642, #7075 ) ;
#6629 = DIRECTION ( 'NONE',  ( 0.000000000000000000, 0.000000000000000000, -1.000000000000000000 ) ) ;
#6630 = ORIENTED_EDGE ( 'NONE', *, *, #3657, .T. ) ;
#6631 = CC_DESIGN_APPROVAL ( #4508, ( #1882 ) ) ;
#6632 = CARTESIAN_POINT ( 'NONE',  ( -0.7335700379171464780, 2.500000000182677873, -2.908930215554831999 ) ) ;
#6633 = CYLINDRICAL_SURFACE ( 'NONE', #5977, 0.1875000000000006661 ) ;
#6634 = CARTESIAN_POINT ( 'NONE',  ( -2.537500000000000533, 2.500000000000000444, 0.2625000000000008438 ) ) ;
#6635 = VERTEX_POINT ( 'NONE', #6951 ) ;
#6636 = PERSON_AND_ORGANIZATION_ROLE ( 'classification_officer' ) ;
#6637 = PLANE ( 'NONE',  #2827 ) ;
#6638 = APPROVAL ( #1038, 'UNSPECIFIED' ) ;
#6639 = ORIENTED_EDGE ( 'NONE', *, *, #4329, .F. ) ;
#6640 = VECTOR ( 'NONE', #4539, 39.37007874015748143 ) ;
#6641 = DIRECTION ( 'NONE',  ( 0.000000000000000000, -1.000000000000000000, 0.000000000000000000 ) ) ;
#6642 = ORIENTED_EDGE ( 'NONE', *, *, #252, .T. ) ;
#6643 = DIRECTION ( 'NONE',  ( 0.000000000000000000, 0.000000000000000000, -1.000000000000000000 ) ) ;
#6644 = ORIENTED_EDGE ( 'NONE', *, *, #501, .F. ) ;
#6645 = APPROVAL_STATUS ( 'not_yet_approved' ) ;
#6646 = DIRECTION ( 'NONE',  ( 0.000000000000000000, 0.000000000000000000, -1.000000000000000000 ) ) ;
#6647 = DATE_AND_TIME ( #7949, #7902 ) ;
#6648 = VERTEX_POINT ( 'NONE', #3145 ) ;
#6649 = AXIS2_PLACEMENT_3D ( 'NONE', #3010, #4820, #8029 ) ;
#6650 = EDGE_CURVE ( 'NONE', #2357, #1469, #7703, .T. ) ;
#6651 = LINE ( 'NONE', #5356, #3706 ) ;
#6652 =( BOUNDED_CURVE ( )  B_SPLINE_CURVE ( 3, ( #2348, #6071, #1076, #2907 ),
 .UNSPECIFIED., .F., .F. ) 
 B_SPLINE_CURVE_WITH_KNOTS ( ( 4, 4 ),
 ( 0.000000000000000000, 1.000000000000000000 ),
 .UNSPECIFIED. ) 
 CURVE ( )  GEOMETRIC_REPRESENTATION_ITEM ( )  RATIONAL_B_SPLINE_CURVE ( ( 1.000000000000000000, 0.3333333333333334259, 0.3333333333333334259, 1.000000000000000000 ) ) 
 REPRESENTATION_ITEM ( '' )  );
#6653 = FACE_OUTER_BOUND ( 'NONE', #657, .T. ) ;
#6654 = AXIS2_PLACEMENT_3D ( 'NONE', #3026, #4386, #697 ) ;
#6655 = DIRECTION ( 'NONE',  ( 0.000000000000000000, -1.000000000000000000, 0.000000000000000000 ) ) ;
#6656 = DATE_TIME_ROLE ( 'classification_date' ) ;
#6657 = EDGE_LOOP ( 'NONE', ( #1352, #1177, #80, #7895 ) ) ;
#6658 = DIRECTION ( 'NONE',  ( 0.000000000000000000, 1.000000000000000000, 0.000000000000000000 ) ) ;
#6659 = EDGE_CURVE ( 'NONE', #1295, #7244, #97, .T. ) ;
#6660 = DIRECTION ( 'NONE',  ( 0.000000000000000000, -0.000000000000000000, 1.000000000000000000 ) ) ;
#6661 = DIRECTION ( 'NONE',  ( 0.000000000000000000, 0.000000000000000000, -1.000000000000000000 ) ) ;
#6662 = CARTESIAN_POINT ( 'NONE',  ( 2.749999999999999556, 7.964000000000000412, 5.236250000000000071 ) ) ;
#6663 = DIRECTION ( 'NONE',  ( -0.000000000000000000, 1.000000000000000000, 0.000000000000000000 ) ) ;
#6664 = CARTESIAN_POINT ( 'NONE',  ( -1.187500000000000000, 5.969165905511811587, 6.858307716535433585 ) ) ;
#6665 = EDGE_LOOP ( 'NONE', ( #3418, #1292 ) ) ;
#6666 = CARTESIAN_POINT ( 'NONE',  ( -3.987046614173228587, 3.900888680994070157, 8.039351542753340851 ) ) ;
#6667 = CARTESIAN_POINT ( 'NONE',  ( -1.625000000000000222, 2.500000000000000444, -2.750000000000000444 ) ) ;
#6668 = ADVANCED_FACE ( 'NONE', ( #6382 ), #2653, .F. ) ;
#6669 = LOCAL_TIME ( 0, 37, 23.00000000000000000, #203 ) ;
#6670 = DIRECTION ( 'NONE',  ( 0.000000000000000000, 0.000000000000000000, 1.000000000000000000 ) ) ;
#6671 = ORIENTED_EDGE ( 'NONE', *, *, #6405, .F. ) ;
#6672 = PERSON_AND_ORGANIZATION ( #7862, #8117 ) ;
#6673 = PLANE ( 'NONE',  #3214 ) ;
#6674 = DATE_TIME_ROLE ( 'classification_date' ) ;
#6675 = CARTESIAN_POINT ( 'NONE',  ( 0.6907419235105254351, 4.242221832517436120, 8.342451301701874655 ) ) ;
#6676 = CYLINDRICAL_SURFACE ( 'NONE', #3751, 1.124999999999999556 ) ;
#6677 = ORIENTED_EDGE ( 'NONE', *, *, #7788, .T. ) ;
#6678 = ORIENTED_EDGE ( 'NONE', *, *, #379, .T. ) ;
#6679 = CARTESIAN_POINT ( 'NONE',  ( -3.987046614173229031, 3.674333370316265501, 7.679916707260901809 ) ) ;
#6680 = VERTEX_POINT ( 'NONE', #4448 ) ;
#6681 = PERSON_AND_ORGANIZATION_ROLE ( 'classification_officer' ) ;
#6682 = CC_DESIGN_DATE_AND_TIME_ASSIGNMENT ( #2335, #6216, ( #1579 ) ) ;
#6683 = CARTESIAN_POINT ( 'NONE',  ( 3.987953385826771946, 4.225666661560477877, 8.782583289749322120 ) ) ;
#6684 = ORIENTED_EDGE ( 'NONE', *, *, #8148, .F. ) ;
#6685 = FACE_OUTER_BOUND ( 'NONE', #5174, .T. ) ;
#6686 = CARTESIAN_POINT ( 'NONE',  ( -0.8651000672161062166, 4.937992838626295011, -5.108750000000002345 ) ) ;
#6687 = CARTESIAN_POINT ( 'NONE',  ( -4.066213280839896527, 4.383999996532201848, 8.231249998505111520 ) ) ;
#6688 = CARTESIAN_POINT ( 'NONE',  ( -0.7122963468828452660, 4.185277942229626902, 8.024595996655373042 ) ) ;
#6689 = SHAPE_REPRESENTATION_RELATIONSHIP ( 'NONE' , 'NONE' ,  #6762, #4162 ) ;
#6690 = CARTESIAN_POINT ( 'NONE',  ( -3.583510604133041344, 1.543025754838327046, 4.388534791062126923E-16 ) ) ;
#6691 = PERSON_AND_ORGANIZATION_ROLE ( 'creator' ) ;
#6692 = VERTEX_POINT ( 'NONE', #136 ) ;
#6693 = CARTESIAN_POINT ( 'NONE',  ( 3.875000000000000000, 1.000000000000000222, -7.750000000000002665 ) ) ;
#6694 = LINE ( 'NONE', #261, #4888 ) ;
#6695 = DIRECTION ( 'NONE',  ( 0.000000000000000000, 0.000000000000000000, -1.000000000000000000 ) ) ;
#6696 = ADVANCED_FACE ( 'NONE', ( #647 ), #7639, .T. ) ;
#6697 = ORIENTED_EDGE ( 'NONE', *, *, #4250, .F. ) ;
#6698 = CYLINDRICAL_SURFACE ( 'NONE', #2527, 2.619834133858267577 ) ;
#6699 = ORIENTED_EDGE ( 'NONE', *, *, #7929, .F. ) ;
#6700 = B_SPLINE_CURVE_WITH_KNOTS ( 'NONE', 3,
 ( #736, #4416, #1307, #7570, #2580, #4376 ),
 .UNSPECIFIED., .F., .F.,
 ( 4, 2, 4 ),
 ( 0.000000000000000000, 0.5000000000000000000, 1.000000000000000000 ),
 .UNSPECIFIED. ) ;
#6701 = DIRECTION ( 'NONE',  ( 1.986798540846736797E-16, 0.000000000000000000, 1.000000000000000000 ) ) ;
#6702 = CARTESIAN_POINT ( 'NONE',  ( -2.875000000000000888, 1.000000000000000222, -2.975000000000000977 ) ) ;
#6703 = LINE ( 'NONE', #4277, #2547 ) ;
#6704 = FACE_OUTER_BOUND ( 'NONE', #101, .T. ) ;
#6705 = ORIENTED_EDGE ( 'NONE', *, *, #3211, .F. ) ;
#6706 = APPROVAL_ROLE ( '' ) ;
#6707 = CARTESIAN_POINT ( 'NONE',  ( -3.987046614173228587, 3.950000015938371689, 8.543749986456024459 ) ) ;
#6708 = CARTESIAN_POINT ( 'NONE',  ( -2.740000000000001545, 8.729000000000002757, 4.313750000000002416 ) ) ;
#6709 = EDGE_CURVE ( 'NONE', #2620, #3365, #4367, .T. ) ;
#6710 =( BOUNDED_CURVE ( )  B_SPLINE_CURVE ( 2, ( #1309, #6882, #6961, #775, #3800, #1396, #3767, #1346, #654 ),
 .UNSPECIFIED., .F., .F. ) 
 B_SPLINE_CURVE_WITH_KNOTS ( ( 3, 2, 2, 2, 3 ),
 ( 1.913691129756523449E-11, 0.004098851392691885663, 0.03173539258822634379, 0.05937193378376098146, 0.07317982563254910033 ),
 .UNSPECIFIED. ) 
 CURVE ( )  GEOMETRIC_REPRESENTATION_ITEM ( )  RATIONAL_B_SPLINE_CURVE ( ( 0.9260057553135141450, 0.9565602018087399072, 1.000000000000000000, 0.7071067811865479058, 1.000000000000000000, 0.7071067811865479058, 1.000000000000000000, 0.8536633850130399548, 0.8535534732088591037 ) ) 
 REPRESENTATION_ITEM ( '' )  );
#6711 = ORIENTED_EDGE ( 'NONE', *, *, #6896, .F. ) ;
#6712 = FACE_OUTER_BOUND ( 'NONE', #5496, .T. ) ;
#6713 = EDGE_LOOP ( 'NONE', ( #6314, #1677, #2155, #2291 ) ) ;
#6714 = CALENDAR_DATE ( 2026, 8, 10 ) ;
#6715 = CARTESIAN_POINT ( 'NONE',  ( 4.067120052493438997, 3.516000035344542418, 9.099249959692771839 ) ) ;
#6716 = ITEM_DEFINED_TRANSFORMATION ( 'NONE', 'NONE', #4510,  #7272 ) ;
#6717 = ORIENTED_EDGE ( 'NONE', *, *, #791, .F. ) ;
#6718 = VECTOR ( 'NONE', #1855, 39.37007874015748143 ) ;
#6719 = VECTOR ( 'NONE', #6509, 39.37007874015748143 ) ;
#6720 = CC_DESIGN_SECURITY_CLASSIFICATION ( #7249, ( #4347 ) ) ;
#6721 = LINE ( 'NONE', #4832, #5800 ) ;
#6722 = CARTESIAN_POINT ( 'NONE',  ( 2.750000000000000888, 7.974000000000001087, 3.823750000000002647 ) ) ;
#6723 =( LENGTH_UNIT ( ) NAMED_UNIT ( * ) SI_UNIT ( $, .METRE. ) );
#6724 = CARTESIAN_POINT ( 'NONE',  ( 2.875000000000000888, -3.820994292482255198E-18, -2.612499998777286780 ) ) ;
#6725 = VECTOR ( 'NONE', #958, 39.37007874015748143 ) ;
#6726 = APPROVAL_ROLE ( '' ) ;
#6727 = ORIENTED_EDGE ( 'NONE', *, *, #5333, .F. ) ;
#6728 = VECTOR ( 'NONE', #3094, 39.37007874015748143 ) ;
#6729 = LINE ( 'NONE', #1118, #7319 ) ;
#6730 = APPROVAL_PERSON_ORGANIZATION ( #5378, #3812, #1743 ) ;
#6731 = CC_DESIGN_DATE_AND_TIME_ASSIGNMENT ( #5677, #7163, ( #7249 ) ) ;
#6732 = VECTOR ( 'NONE', #6148, 39.37007874015748143 ) ;
#6733 = CARTESIAN_POINT ( 'NONE',  ( -3.063407153088590462, 2.250083286718937536, -0.5624999982030005619 ) ) ;
#6734 = DIRECTION ( 'NONE',  ( -0.000000000000000000, -0.000000000000000000, -1.000000000000000000 ) ) ;
#6735 = CARTESIAN_POINT ( 'NONE',  ( 0.000000000000000000, 5.376007322834645663, 5.972081456692916568 ) ) ;
#6736 = VERTEX_POINT ( 'NONE', #3223 ) ;
#6737 = PLANE ( 'NONE',  #24 ) ;
#6738 = ORIENTED_EDGE ( 'NONE', *, *, #2346, .F. ) ;
#6739 = AXIS2_PLACEMENT_3D ( 'NONE', #985, #3480, #7772 ) ;
#6740 = EDGE_CURVE ( 'NONE', #750, #2216, #7603, .T. ) ;
#6741 = CARTESIAN_POINT ( 'NONE',  ( -2.745000000000000995, 7.973999999999999311, 4.318750000000002309 ) ) ;
#6742 = DIRECTION ( 'NONE',  ( -1.000000000000000000, -0.000000000000000000, -0.000000000000000000 ) ) ;
#6743 = CLOSED_SHELL ( 'NONE', ( #6555, #2379, #5785, #2999, #4779, #5069, #6563, #7849, #7475, #959 ) ) ;
#6744 = FACE_OUTER_BOUND ( 'NONE', #2702, .T. ) ;
#6745 = AXIS2_PLACEMENT_3D ( 'NONE', #5150, #7698, #7822 ) ;
#6746 = PRODUCT ( 'bench vise4-', 'bench vise4-', '', ( #7273 ) ) ;
#6747 = PLANE ( 'NONE',  #3060 ) ;
#6748 = CARTESIAN_POINT ( 'NONE',  ( -1.625000000000000222, 2.500000000077463369, -2.521780125186765975 ) ) ;
#6749 = VERTEX_POINT ( 'NONE', #6871 ) ;
#6750 = PERSON_AND_ORGANIZATION ( #7862, #8117 ) ;
#6751 = VECTOR ( 'NONE', #4531, 39.37007874015748854 ) ;
#6752 = AXIS2_PLACEMENT_3D ( 'NONE', #1010, #971, #5374 ) ;
#6753 = ORIENTED_EDGE ( 'NONE', *, *, #6772, .T. ) ;
#6754 = FACE_OUTER_BOUND ( 'NONE', #6590, .T. ) ;
#6755 = CARTESIAN_POINT ( 'NONE',  ( -3.987046614173229031, 3.753500037802126599, 7.838250042232624004 ) ) ;
#6756 = ADVANCED_FACE ( 'NONE', ( #5801 ), #1387, .T. ) ;
#6757 = EDGE_LOOP ( 'NONE', ( #1682, #6364, #7888, #6727 ) ) ;
#6758 = ADVANCED_FACE ( 'NONE', ( #3758 ), #6259, .T. ) ;
#6759 = APPROVAL_ROLE ( '' ) ;
#6760 = PLANE ( 'NONE',  #2940 ) ;
#6761 = SECURITY_CLASSIFICATION_LEVEL ( 'unclassified' ) ;
#6762 = SHAPE_REPRESENTATION ( 'bench vise4-', ( #7272 ), #1120 ) ;
#6763 = ADVANCED_FACE ( 'NONE', ( #7564 ), #2078, .F. ) ;
#6764 = CARTESIAN_POINT ( 'NONE',  ( 0.000000000000000000, 5.541000000000003034, 3.956250000000000266 ) ) ;
#6765 = LINE ( 'NONE', #6837, #5303 ) ;
#6766 = VERTEX_POINT ( 'NONE', #4727 ) ;
#6767 = CARTESIAN_POINT ( 'NONE',  ( -4.462046614173230452, 3.674333370316265057, 8.782583289749325672 ) ) ;
#6768 = PLANE ( 'NONE',  #452 ) ;
#6769 = AXIS2_PLACEMENT_3D ( 'NONE', #1175, #4938, #7481 ) ;
#6770 = PERSON_AND_ORGANIZATION ( #7862, #8117 ) ;
#6771 = EDGE_LOOP ( 'NONE', ( #7680, #7623, #7585, #2915 ) ) ;
#6772 = EDGE_CURVE ( 'NONE', #789, #5413, #4570, .T. ) ;
#6773 = EDGE_LOOP ( 'NONE', ( #3942, #5250, #4001, #3075, #4672, #7484, #665, #4338, #4069, #2279 ) ) ;
#6774 = DIRECTION ( 'NONE',  ( 0.000000000000000000, 0.000000000000000000, 1.000000000000000000 ) ) ;
#6775 = DIRECTION ( 'NONE',  ( 0.9917930140014037388, 0.000000000000000000, 0.1278538907425630367 ) ) ;
#6776 = ORIENTED_EDGE ( 'NONE', *, *, #6659, .F. ) ;
#6777 = CC_DESIGN_PERSON_AND_ORGANIZATION_ASSIGNMENT ( #7576, #6313, ( #3856 ) ) ;
#6778 = LINE ( 'NONE', #5368, #6061 ) ;
#6779 = ORIENTED_EDGE ( 'NONE', *, *, #921, .T. ) ;
#6780 = DIRECTION ( 'NONE',  ( -0.000000000000000000, -1.000000000000000000, -0.000000000000000000 ) ) ;
#6781 = FACE_OUTER_BOUND ( 'NONE', #1813, .T. ) ;
#6782 = LINE ( 'NONE', #4767, #3457 ) ;
#6783 = CARTESIAN_POINT ( 'NONE',  ( 1.187500000000000444, 4.913748861513248301, 4.936700916451632004 ) ) ;
#6784 = VERTEX_POINT ( 'NONE', #3989 ) ;
#6785 = PERSON_AND_ORGANIZATION ( #7862, #8117 ) ;
#6786 = DIRECTION ( 'NONE',  ( -0.000000000000000000, 1.000000000000000000, -0.000000000000000000 ) ) ;
#6787 = EDGE_CURVE ( 'NONE', #2209, #6810, #2851, .T. ) ;
#6788 = EDGE_LOOP ( 'NONE', ( #4863, #7890, #3539, #783, #7940, #2736 ) ) ;
#6789 = ADVANCED_FACE ( 'NONE', ( #7122 ), #2202, .F. ) ;
#6790 = FACE_OUTER_BOUND ( 'NONE', #774, .T. ) ;
#6791 = CARTESIAN_POINT ( 'NONE',  ( -3.987046614173228587, 3.753500037802127043, 8.231249998505111520 ) ) ;
#6792 = CARTESIAN_POINT ( 'NONE',  ( 2.750000000000000444, 8.719000000000002970, 4.313750000000002416 ) ) ;
#6793 = EDGE_LOOP ( 'NONE', ( #5370, #339, #5114, #4796 ) ) ;
#6794 = CALENDAR_DATE ( 2026, 8, 10 ) ;
#6795 = ADVANCED_FACE ( 'NONE', ( #7080 ), #3938, .F. ) ;
#6796 = DIRECTION ( 'NONE',  ( 0.000000000000000000, -1.000000000000000000, 0.000000000000000000 ) ) ;
#6797 = APPROVAL_DATE_TIME ( #4293, #1614 ) ;
#6798 = LINE ( 'NONE', #1872, #75 ) ;
#6799 = CARTESIAN_POINT ( 'NONE',  ( 1.198957881665148717, 2.500000000196656025, -2.749999999536767437 ) ) ;
#6800 = DIRECTION ( 'NONE',  ( -0.7071067811865475727, -0.7071067811865475727, 0.000000000000000000 ) ) ;
#6801 = FACE_OUTER_BOUND ( 'NONE', #737, .T. ) ;
#6802 = ORIENTED_EDGE ( 'NONE', *, *, #8102, .T. ) ;
#6803 = LINE ( 'NONE', #6722, #6732 ) ;
#6804 = CARTESIAN_POINT ( 'NONE',  ( 2.861675873811764248, 1.000000000000000222, -2.612744953730403719 ) ) ;
#6805 = CALENDAR_DATE ( 2026, 8, 10 ) ;
#6806 = ORIENTED_EDGE ( 'NONE', *, *, #3974, .T. ) ;
#6807 = CARTESIAN_POINT ( 'NONE',  ( -2.750000000000000444, 7.964000000000000412, 4.313750000000002416 ) ) ;
#6808 = EDGE_CURVE ( 'NONE', #1666, #8086, #2114, .T. ) ;
#6809 = PRODUCT ( 'bench vise10-', 'bench vise10-', '', ( #8179 ) ) ;
#6810 = VERTEX_POINT ( 'NONE', #5887 ) ;
#6811 = DIRECTION ( 'NONE',  ( -0.000000000000000000, -0.000000000000000000, 1.000000000000000000 ) ) ;
#6812 = LINE ( 'NONE', #8185, #6475 ) ;
#6813 = CC_DESIGN_APPROVAL ( #6214, ( #5099 ) ) ;
#6814 = CARTESIAN_POINT ( 'NONE',  ( 0.000000000000000000, 5.113999999999999879, -2.750000000000000444 ) ) ;
#6815 = VERTEX_POINT ( 'NONE', #889 ) ;
#6816 = EDGE_LOOP ( 'NONE', ( #5528, #777, #4306, #1254 ) ) ;
#6817 = ADVANCED_BREP_SHAPE_REPRESENTATION ( '', ( #4468, #7272 ), #720 ) ;
#6818 = CARTESIAN_POINT ( 'NONE',  ( -1.625000000000000222, 5.639000000000001123, -2.750000000000000444 ) ) ;
#6819 = DIRECTION ( 'NONE',  ( 1.000000000000000000, 0.000000000000000000, 0.000000000000000000 ) ) ;
#6820 = CARTESIAN_POINT ( 'NONE',  ( 1.187500000000000000, 4.660936287869686723, 6.010159138129464118 ) ) ;
#6821 = ORIENTED_EDGE ( 'NONE', *, *, #3268, .T. ) ;
#6822 = COORDINATED_UNIVERSAL_TIME_OFFSET ( 0, 0, .AHEAD. ) ;
#6823 = LINE ( 'NONE', #5713, #2838 ) ;
#6824 = CC_DESIGN_PERSON_AND_ORGANIZATION_ASSIGNMENT ( #6672, #4106, ( #303 ) ) ;
#6825 = DIRECTION ( 'NONE',  ( 0.000000000000000000, 0.000000000000000000, -1.000000000000000000 ) ) ;
#6826 = DIRECTION ( 'NONE',  ( -0.9917930140014037388, 0.000000000000000000, -0.1278538907425633420 ) ) ;
#6827 = DIRECTION ( 'NONE',  ( -0.000000000000000000, -0.000000000000000000, 1.000000000000000000 ) ) ;
#6828 = ORIENTED_EDGE ( 'NONE', *, *, #3732, .F. ) ;
#6829 = APPROVAL_DATE_TIME ( #7485, #666 ) ;
#6830 = CARTESIAN_POINT ( 'NONE',  ( -1.312500000000000222, 8.589000000000002188, 3.161250000126027970 ) ) ;
#6831 = EDGE_CURVE ( 'NONE', #6974, #2706, #6597, .T. ) ;
#6832 = SECURITY_CLASSIFICATION_LEVEL ( 'unclassified' ) ;
#6833 = LINE ( 'NONE', #1216, #4274 ) ;
#6834 = ADVANCED_FACE ( 'NONE', ( #2157 ), #975, .T. ) ;
#6835 = EDGE_CURVE ( 'NONE', #7577, #2826, #7726, .T. ) ;
#6836 = CARTESIAN_POINT ( 'NONE',  ( -1.312500000000000444, 5.414000000000000590, 0.5414159055118118458 ) ) ;
#6837 = CARTESIAN_POINT ( 'NONE',  ( 2.740000000000000213, 8.724000000000001975, 3.818750000000003197 ) ) ;
#6838 = CARTESIAN_POINT ( 'NONE',  ( -3.343750000000001776, 2.500000000000000444, 0.5625000000000001110 ) ) ;
#6839 = ORIENTED_EDGE ( 'NONE', *, *, #7928, .F. ) ;
#6840 = CARTESIAN_POINT ( 'NONE',  ( -0.7077600209949282961, 4.198434470451293699, 8.421896151506285122 ) ) ;
#6841 = DIRECTION ( 'NONE',  ( 1.000000000000000000, 0.000000000000000000, 0.000000000000000000 ) ) ;
#6842 = CARTESIAN_POINT ( 'NONE',  ( -1.624999999999999778, 3.950000000000000178, 3.691250000234376216 ) ) ;
#6843 = PERSON_AND_ORGANIZATION ( #7862, #8117 ) ;
#6844 = ORIENTED_EDGE ( 'NONE', *, *, #1427, .T. ) ;
#6845 = VECTOR ( 'NONE', #3579, 39.37007874015748143 ) ;
#6846 = LOCAL_TIME ( 0, 37, 23.00000000000000000, #2696 ) ;
#6847 = ORIENTED_EDGE ( 'NONE', *, *, #6360, .F. ) ;
#6848 = DIRECTION ( 'NONE',  ( 0.000000000000000000, 0.000000000000000000, -1.000000000000000000 ) ) ;
#6849 = EDGE_CURVE ( 'NONE', #7757, #7088, #5340, .T. ) ;
#6850 = ADVANCED_FACE ( 'N', ( #5970 ), #6559, .T. ) ;
#6851 = ORIENTED_EDGE ( 'NONE', *, *, #7373, .F. ) ;
#6852 =( BOUNDED_CURVE ( )  B_SPLINE_CURVE ( 3, ( #7744, #2096, #5868, #6764 ),
 .UNSPECIFIED., .F., .F. ) 
 B_SPLINE_CURVE_WITH_KNOTS ( ( 4, 4 ),
 ( 0.000000000000000000, 1.000000000000000000 ),
 .UNSPECIFIED. ) 
 CURVE ( )  GEOMETRIC_REPRESENTATION_ITEM ( )  RATIONAL_B_SPLINE_CURVE ( ( 1.000000000000000000, 0.8047378541243660477, 0.8047378541243660477, 1.000000000000000000 ) ) 
 REPRESENTATION_ITEM ( '' )  );
#6853 = ORIENTED_EDGE ( 'NONE', *, *, #1468, .T. ) ;
#6854 = AXIS2_PLACEMENT_3D ( 'NONE', #4142, #6701, #1620 ) ;
#6855 =( REPRESENTATION_RELATIONSHIP ('NONE','NONE', #3256, #6762 ) REPRESENTATION_RELATIONSHIP_WITH_TRANSFORMATION ( #3716 )SHAPE_REPRESENTATION_RELATIONSHIP( ) );
#6856 = CARTESIAN_POINT ( 'NONE',  ( 3.987953385826772390, 4.121369605928006052, 8.135040162505021044 ) ) ;
#6857 = DIRECTION ( 'NONE',  ( 0.7071067811865474617, -0.000000000000000000, -0.7071067811865474617 ) ) ;
#6858 = FACE_OUTER_BOUND ( 'NONE', #6583, .T. ) ;
#6859 = VERTEX_POINT ( 'NONE', #2239 ) ;
#6860 = DATE_AND_TIME ( #4352, #1363 ) ;
#6861 = PLANE ( 'NONE',  #5443 ) ;
#6862 = AXIS2_PLACEMENT_3D ( 'NONE', #1237, #6894, #6933 ) ;
#6863 = ORIENTED_EDGE ( 'NONE', *, *, #5957, .T. ) ;
#6864 = AXIS2_PLACEMENT_3D ( 'NONE', #5557, #5435, #1719 ) ;
#6865 = CIRCLE ( 'NONE', #6739, 0.1875000000000006661 ) ;
#6866 = FACE_OUTER_BOUND ( 'NONE', #1199, .T. ) ;
#6867 = CARTESIAN_POINT ( 'NONE',  ( 1.187500000000000444, 7.339000000000001300, 4.486250000000000959 ) ) ;
#6868 = DIRECTION ( 'NONE',  ( 0.000000000000000000, 0.000000000000000000, -1.000000000000000000 ) ) ;
#6869 = ORIENTED_EDGE ( 'NONE', *, *, #4247, .F. ) ;
#6870 = CALENDAR_DATE ( 2026, 8, 10 ) ;
#6871 = CARTESIAN_POINT ( 'NONE',  ( 2.537500000000000533, 1.664000000000000368, -0.2625000000000008438 ) ) ;
#6872 = AXIS2_PLACEMENT_3D ( 'NONE', #9, #2532, #5019 ) ;
#6873 = APPROVAL_STATUS ( 'not_yet_approved' ) ;
#6874 = APPROVAL ( #3493, 'UNSPECIFIED' ) ;
#6875 = CARTESIAN_POINT ( 'NONE',  ( -6.890193713091687007E-11, 5.025000000000000355, 3.440250000000001140 ) ) ;
#6876 = CARTESIAN_POINT ( 'NONE',  ( 2.750000000000000444, 7.964000000000000412, 5.246694173228347857 ) ) ;
#6877 = VECTOR ( 'NONE', #7763, 39.37007874015748854 ) ;
#6878 = DIRECTION ( 'NONE',  ( 0.000000000000000000, 0.000000000000000000, 1.000000000000000000 ) ) ;
#6879 = CARTESIAN_POINT ( 'NONE',  ( 0.000000000000000000, 8.523567361303525658, 4.820336052022350160 ) ) ;
#6880 = LINE ( 'NONE', #6922, #164 ) ;
#6881 = ORIENTED_EDGE ( 'NONE', *, *, #1468, .F. ) ;
#6882 = CARTESIAN_POINT ( 'NONE',  ( -2.750000000000000444, 8.589000000000000412, 4.404023385826772774 ) ) ;
#6883 = CARTESIAN_POINT ( 'NONE',  ( -1.187500000000000888, 4.211027880314613725, 6.838140405204945260 ) ) ;
#6884 = PERSON_AND_ORGANIZATION ( #7862, #8117 ) ;
#6885 = ORIENTED_EDGE ( 'NONE', *, *, #3696, .F. ) ;
#6886 = EDGE_CURVE ( 'NONE', #1945, #1578, #4688, .T. ) ;
#6887 = DIRECTION ( 'NONE',  ( -1.000000000000000000, 0.000000000000000000, -0.000000000000000000 ) ) ;
#6888 = VECTOR ( 'NONE', #4005, 39.37007874015748143 ) ;
#6889 = EDGE_CURVE ( 'NONE', #6749, #5733, #2767, .T. ) ;
#6890 = EDGE_CURVE ( 'NONE', #4253, #3252, #1549, .T. ) ;
#6891 = DIRECTION ( 'NONE',  ( -0.7071067811865474617, -0.7071067811865474617, -0.000000000000000000 ) ) ;
#6892 = CARTESIAN_POINT ( 'NONE',  ( 0.000000000000000000, 3.950000000000000178, -2.750000000000000444 ) ) ;
#6893 = AXIS2_PLACEMENT_3D ( 'NONE', #427, #7293, #6085 ) ;
#6894 = DIRECTION ( 'NONE',  ( -0.000000000000000000, -0.000000000000000000, 1.000000000000000000 ) ) ;
#6895 = VERTEX_POINT ( 'NONE', #4108 ) ;
#6896 = EDGE_CURVE ( 'NONE', #1742, #1901, #927, .T. ) ;
#6897 = ORIENTED_EDGE ( 'NONE', *, *, #5629, .T. ) ;
#6898 = VECTOR ( 'NONE', #2656, 39.37007874015748143 ) ;
#6899 = VECTOR ( 'NONE', #3568, 39.37007874015748143 ) ;
#6900 = ADVANCED_FACE ( 'NONE', ( #233 ), #6637, .F. ) ;
#6901 = CARTESIAN_POINT ( 'NONE',  ( 0.000000000000000000, 2.500000000000000444, -2.749999999536767437 ) ) ;
#6902 = CARTESIAN_POINT ( 'NONE',  ( 1.312363190093051912, 3.862340101006792814, -5.108750000000001457 ) ) ;
#6903 = CARTESIAN_POINT ( 'NONE',  ( 3.651126735575231042, 1.000000000000000222, -1.298036422080803165 ) ) ;
#6904 = ORIENTED_EDGE ( 'NONE', *, *, #4038, .F. ) ;
#6905 = APPROVAL_ROLE ( '' ) ;
#6906 = CARTESIAN_POINT ( 'NONE',  ( -1.462953685906409840, 1.000000000000000222, 3.588229579118171308 ) ) ;
#6907 = ORIENTED_EDGE ( 'NONE', *, *, #237, .T. ) ;
#6908 = ADVANCED_FACE ( 'NONE', ( #7340 ), #1091, .F. ) ;
#6909 = LOCAL_TIME ( 0, 37, 23.00000000000000000, #4995 ) ;
#6910 = LINE ( 'NONE', #3295, #7973 ) ;
#6911 = CARTESIAN_POINT ( 'NONE',  ( 0.000000000000000000, 5.541000000000003034, 3.956250000000000266 ) ) ;
#6912 = VERTEX_POINT ( 'NONE', #6207 ) ;
#6913 = APPROVAL_DATE_TIME ( #3757, #7084 ) ;
#6914 = CARTESIAN_POINT ( 'NONE',  ( 4.462953385826771147, 3.753500037802128375, 8.231249998505111520 ) ) ;
#6915 = CONTEXT_DEPENDENT_SHAPE_REPRESENTATION ( #6445, #3080 ) ;
#6916 = DIRECTION ( 'NONE',  ( -0.7071067811865474617, 0.7071067811865474617, -0.000000000000000000 ) ) ;
#6917 = CARTESIAN_POINT ( 'NONE',  ( 2.740000000000001545, 8.729000000000002757, 3.823750000000002647 ) ) ;
#6918 = LOCAL_TIME ( 0, 37, 23.00000000000000000, #1476 ) ;
#6919 = CARTESIAN_POINT ( 'NONE',  ( -3.987046614173229475, 3.823364637257366638, 8.080727712660298323 ) ) ;
#6920 = CARTESIAN_POINT ( 'NONE',  ( -8.751021560936518753E-10, 1.365923996832131609E-16, 5.750408897959578548E-10 ) ) ;
#6921 = CC_DESIGN_PERSON_AND_ORGANIZATION_ASSIGNMENT ( #1681, #7394, ( #5099 ) ) ;
#6922 = CARTESIAN_POINT ( 'NONE',  ( 1.625000000000000222, 5.113999999999999879, 2.750000000000000444 ) ) ;
#6923 = ORIENTED_EDGE ( 'NONE', *, *, #6201, .T. ) ;
#6924 = CARTESIAN_POINT ( 'NONE',  ( -3.987046614173228587, 3.753500037802127043, 8.231249998505111520 ) ) ;
#6925 = SHAPE_REPRESENTATION ( 'bench vise8-', ( #7272 ), #1513 ) ;
#6926 = CARTESIAN_POINT ( 'NONE',  ( 2.750000000000000444, 8.589000000000000412, 4.486250000000000959 ) ) ;
#6927 = DATE_AND_TIME ( #2624, #3890 ) ;
#6928 = VERTEX_POINT ( 'NONE', #1744 ) ;
#6929 = EDGE_CURVE ( 'NONE', #3899, #3397, #7301, .T. ) ;
#6930 = FACE_OUTER_BOUND ( 'NONE', #2135, .T. ) ;
#6931 = ADVANCED_FACE ( 'NONE', ( #1056 ), #6673, .F. ) ;
#6932 = DIRECTION ( 'NONE',  ( 1.000000000000000000, 0.000000000000000000, 0.000000000000000000 ) ) ;
#6933 = DIRECTION ( 'NONE',  ( 1.000000000000000000, 0.000000000000000000, 0.000000000000000000 ) ) ;
#6934 = CARTESIAN_POINT ( 'NONE',  ( 3.343750000000001776, 1.750000000000000444, 0.5624999982029994516 ) ) ;
#6935 = EDGE_LOOP ( 'NONE', ( #4656, #1198, #1287, #7702 ) ) ;
#6936 = ORIENTED_EDGE ( 'NONE', *, *, #3243, .F. ) ;
#6937 = LOCAL_TIME ( 0, 37, 23.00000000000000000, #6058 ) ;
#6938 = EDGE_CURVE ( 'NONE', #5487, #4455, #4816, .T. ) ;
#6939 = CARTESIAN_POINT ( 'NONE',  ( 3.987953385826772390, 3.880579470499919026, 8.047419037877352466 ) ) ;
#6940 = CARTESIAN_POINT ( 'NONE',  ( 1.261644055928290875, 3.587548275720691571, -5.108750000000004121 ) ) ;
#6941 = CARTESIAN_POINT ( 'NONE',  ( -2.740000000000000213, 8.719000000000001194, 3.323750000000001759 ) ) ;
#6942 = VERTEX_POINT ( 'NONE', #547 ) ;
#6943 = LOCAL_TIME ( 0, 37, 23.00000000000000000, #7383 ) ;
#6944 = CARTESIAN_POINT ( 'NONE',  ( 3.987953385826772390, 3.778630425948584559, 8.327459834505681613 ) ) ;
#6945 = VERTEX_POINT ( 'NONE', #8068 ) ;
#6946 = CC_DESIGN_SECURITY_CLASSIFICATION ( #3413, ( #449 ) ) ;
#6947 = DIRECTION ( 'NONE',  ( 0.000000000000000000, 0.7071067811865474617, 0.7071067811865474617 ) ) ;
#6948 = LINE ( 'NONE', #5631, #1504 ) ;
#6949 = EDGE_LOOP ( 'NONE', ( #8066, #5502 ) ) ;
#6950 = SECURITY_CLASSIFICATION_LEVEL ( 'unclassified' ) ;
#6951 = CARTESIAN_POINT ( 'NONE',  ( -2.750000000000000444, 7.973999999999999311, 4.313750000000002416 ) ) ;
#6952 = CALENDAR_DATE ( 2026, 8, 10 ) ;
#6953 = EDGE_CURVE ( 'NONE', #6962, #6912, #6050, .T. ) ;
#6954 = CARTESIAN_POINT ( 'NONE',  ( -1.187499999443275334, 5.002317768720649482, 4.083473622047245399 ) ) ;
#6955 = DIRECTION ( 'NONE',  ( -0.000000000000000000, -0.000000000000000000, 1.000000000000000000 ) ) ;
#6956 = EDGE_CURVE ( 'NONE', #4674, #1699, #1710, .T. ) ;
#6957 = CARTESIAN_POINT ( 'NONE',  ( -0.7499999999999993339, 3.950000000000000178, 8.831250000000000711 ) ) ;
#6958 = CARTESIAN_POINT ( 'NONE',  ( 1.312500000000000444, 8.589000000000002188, 3.161250000147724837 ) ) ;
#6959 = CARTESIAN_POINT ( 'NONE',  ( -2.815000008655331509, 1.365923996832131609E-16, -3.895000002097408487 ) ) ;
#6960 = ORIENTED_EDGE ( 'NONE', *, *, #3242, .F. ) ;
#6961 = CARTESIAN_POINT ( 'NONE',  ( -2.750000000000000444, 8.589000000000000412, 4.486250000000000959 ) ) ;
#6962 = VERTEX_POINT ( 'NONE', #4233 ) ;
#6963 = CARTESIAN_POINT ( 'NONE',  ( 3.362500000000000711, 1.750000000000000444, -4.117874862132976456E-16 ) ) ;
#6964 = DIRECTION ( 'NONE',  ( 0.000000000000000000, 0.000000000000000000, 1.000000000000000000 ) ) ;
#6965 = PERSON_AND_ORGANIZATION_ROLE ( 'design_owner' ) ;
#6966 = VERTEX_POINT ( 'NONE', #5379 ) ;
#6967 = LINE ( 'NONE', #7535, #6377 ) ;
#6968 = APPLICATION_CONTEXT ( 'configuration controlled 3d designs of mechanical parts and assemblies' ) ;
#6969 = SHAPE_REPRESENTATION ( 'bench vise6_3-', ( #7272 ), #3475 ) ;
#6970 = EDGE_CURVE ( 'NONE', #4298, #7385, #7479, .T. ) ;
#6971 = CARTESIAN_POINT ( 'NONE',  ( 0.000000000000000000, 3.950000000000000178, 8.831250000000000711 ) ) ;
#6972 = CARTESIAN_POINT ( 'NONE',  ( -8.751021560936518753E-10, 1.000000000000000222, 5.750408897959578548E-10 ) ) ;
#6973 = FACE_OUTER_BOUND ( 'NONE', #6976, .T. ) ;
#6974 = VERTEX_POINT ( 'NONE', #1172 ) ;
#6975 = CC_DESIGN_APPROVAL ( #7084, ( #7802 ) ) ;
#6976 = EDGE_LOOP ( 'NONE', ( #6397, #4663, #7077, #5741 ) ) ;
#6977 = PRODUCT_RELATED_PRODUCT_CATEGORY ( 'detail', '', ( #8109 ) ) ;
#6978 = VECTOR ( 'NONE', #2880, 39.37007874015748143 ) ;
#6979 = VECTOR ( 'NONE', #412, 39.37007874015748143 ) ;
#6980 = APPROVAL_PERSON_ORGANIZATION ( #4856, #6376, #1135 ) ;
#6981 = ADVANCED_FACE ( 'NONE', ( #2364 ), #4857, .T. ) ;
#6982 = CARTESIAN_POINT ( 'NONE',  ( 3.987953385826772390, 3.879123177173087633, 8.047976087269148593 ) ) ;
#6983 = CARTESIAN_POINT ( 'NONE',  ( 0.5437243537200630028, 5.145354609571764826, -5.108750000000003233 ) ) ;
#6984 = EDGE_CURVE ( 'NONE', #6239, #3049, #6451, .T. ) ;
#6985 = DIRECTION ( 'NONE',  ( -1.000000000000000000, -0.000000000000000000, 0.000000000000000000 ) ) ;
#6986 = VERTEX_POINT ( 'NONE', #3670 ) ;
#6987 = PRODUCT_DEFINITION_SHAPE ( 'NONE', 'NONE',  #8198 ) ;
#6988 = CIRCLE ( 'NONE', #2009, 1.591000000000001080 ) ;
#6989 = EDGE_CURVE ( 'NONE', #6648, #4304, #2403, .T. ) ;
#6990 = CC_DESIGN_SECURITY_CLASSIFICATION ( #2668, ( #2798 ) ) ;
#6991 = AXIS2_PLACEMENT_3D ( 'NONE', #2399, #389, #6047 ) ;
#6992 = CIRCLE ( 'NONE', #5545, 0.3625000000000019318 ) ;
#6993 = CARTESIAN_POINT ( 'NONE',  ( 3.562500000000000444, -0.000000000000000000, 2.975000000000000977 ) ) ;
#6994 = PLANE ( 'NONE',  #6086 ) ;
#6995 = ORIENTED_EDGE ( 'NONE', *, *, #7675, .T. ) ;
#6996 = PERSON_AND_ORGANIZATION_ROLE ( 'design_owner' ) ;
#6997 = CARTESIAN_POINT ( 'NONE',  ( -1.625000000000000222, 2.057992047244095346, 2.750000000000000444 ) ) ;
#6998 = PERSON_AND_ORGANIZATION_ROLE ( 'classification_officer' ) ;
#6999 = VECTOR ( 'NONE', #6319, 39.37007874015748143 ) ;
#7000 = VECTOR ( 'NONE', #93, 39.37007874015748854 ) ;
#7001 = ORIENTED_EDGE ( 'NONE', *, *, #3956, .F. ) ;
#7002 = ADVANCED_FACE ( 'NONE', ( #6168 ), #5504, .T. ) ;
#7003 = LINE ( 'NONE', #5106, #702 ) ;
#7004 = EDGE_CURVE ( 'NONE', #2549, #7021, #3862, .T. ) ;
#7005 = DIRECTION ( 'NONE',  ( 1.000000000000000000, 0.000000000000000000, 0.000000000000000000 ) ) ;
#7006 = AXIS2_PLACEMENT_3D ( 'NONE', #5512, #488, #1144 ) ;
#7007 = CARTESIAN_POINT ( 'NONE',  ( -3.987046614173230363, 3.880579470500146844, 8.415080959133112160 ) ) ;
#7008 = ORIENTED_EDGE ( 'NONE', *, *, #5586, .T. ) ;
#7009 = CARTESIAN_POINT ( 'NONE',  ( -4.066213280839894750, 4.383999996532201848, 9.099249959692773615 ) ) ;
#7010 = CARTESIAN_POINT ( 'NONE',  ( 0.000000000000000000, 0.000000000000000000, 0.000000000000000000 ) ) ;
#7011 = CARTESIAN_POINT ( 'NONE',  ( 2.750000000000000888, 8.589000000000000412, 4.404023385826772774 ) ) ;
#7012 = CALENDAR_DATE ( 2026, 8, 10 ) ;
#7013 = EDGE_LOOP ( 'NONE', ( #3658, #2601 ) ) ;
#7014 = DIRECTION ( 'NONE',  ( 1.000000000000000000, 0.000000000000000000, 0.000000000000000000 ) ) ;
#7015 = CIRCLE ( 'NONE', #3984, 0.3625000012227142521 ) ;
#7016 = AXIS2_PLACEMENT_3D ( 'NONE', #5376, #3509, #7932 ) ;
#7017 = DIMENSIONAL_EXPONENTS ( 1.000000000000000000, 0.000000000000000000, 0.000000000000000000, 0.000000000000000000, 0.000000000000000000, 0.000000000000000000, 0.000000000000000000 ) ;
#7018 = CARTESIAN_POINT ( 'NONE',  ( 1.312500000000000444, 5.414000000000000590, 2.750000000234376074 ) ) ;
#7019 = CARTESIAN_POINT ( 'NONE',  ( 1.312500000000000444, 5.414000000000000590, 3.316250000000001474 ) ) ;
#7020 = CARTESIAN_POINT ( 'NONE',  ( -1.074999999999999289, 3.950000000000000178, -4.043750000000001066 ) ) ;
#7021 = VERTEX_POINT ( 'NONE', #2325 ) ;
#7022 = CARTESIAN_POINT ( 'NONE',  ( -0.6994518761186669931, 3.679055344357500701, 8.074232055893794779 ) ) ;
#7023 = CARTESIAN_POINT ( 'NONE',  ( 0.7210596466522596337, 3.743128570366075270, 8.466341326185078842 ) ) ;
#7024 = VERTEX_POINT ( 'NONE', #6707 ) ;
#7025 = UNCERTAINTY_MEASURE_WITH_UNIT (LENGTH_MEASURE( 1.000000000000000082E-05 ), #2479, 'distance_accuracy_value', 'NONE');
#7026 =( BOUNDED_CURVE ( )  B_SPLINE_CURVE ( 3, ( #1225, #1883, #3726, #4256 ),
 .UNSPECIFIED., .F., .F. ) 
 B_SPLINE_CURVE_WITH_KNOTS ( ( 4, 4 ),
 ( 2.728824016688292285E-13, 0.04207438243413257062 ),
 .UNSPECIFIED. ) 
 CURVE ( )  GEOMETRIC_REPRESENTATION_ITEM ( )  RATIONAL_B_SPLINE_CURVE ( ( 0.9996521287660724564, 0.6993327816080832093, 0.5343480788959518168, 0.5046980206296781679 ) ) 
 REPRESENTATION_ITEM ( '' )  );
#7027 = CIRCLE ( 'NONE', #1404, 1.624999999999999778 ) ;
#7028 = CARTESIAN_POINT ( 'NONE',  ( 3.987953385826771058, 3.919106724552877452, 8.036472273046371129 ) ) ;
#7029 = CC_DESIGN_PERSON_AND_ORGANIZATION_ASSIGNMENT ( #416, #531, ( #449 ) ) ;
#7030 = CARTESIAN_POINT ( 'NONE',  ( 0.08777339715507348483, 5.260278687702092171, -5.108750000000001457 ) ) ;
#7031 = LINE ( 'NONE', #7505, #6225 ) ;
#7032 = CARTESIAN_POINT ( 'NONE',  ( 1.187500002638678165, 4.186788052716939212, 6.858307716535433585 ) ) ;
#7033 = ORIENTED_EDGE ( 'NONE', *, *, #675, .T. ) ;
#7034 = DIRECTION ( 'NONE',  ( -0.000000000000000000, -0.000000000000000000, 1.000000000000000000 ) ) ;
#7035 = AXIS2_PLACEMENT_3D ( 'NONE', #1147, #3649, #5560 ) ;
#7036 = ORIENTED_EDGE ( 'NONE', *, *, #6498, .T. ) ;
#7037 = VECTOR ( 'NONE', #2005, 39.37007874015748143 ) ;
#7038 = CYLINDRICAL_SURFACE ( 'NONE', #1651, 0.2625000000000008438 ) ;
#7039 = CARTESIAN_POINT ( 'NONE',  ( 0.000000000000000000, 2.875000000000000444, 3.742515787401575533 ) ) ;
#7040 = ORIENTED_EDGE ( 'NONE', *, *, #3929, .F. ) ;
#7041 = APPROVAL_STATUS ( 'not_yet_approved' ) ;
#7042 = DIRECTION ( 'NONE',  ( 0.000000000000000000, 0.000000000000000000, -1.000000000000000000 ) ) ;
#7043 = FACE_OUTER_BOUND ( 'NONE', #2212, .T. ) ;
#7044 = DIRECTION ( 'NONE',  ( 0.000000000000000000, 0.000000000000000000, 1.000000000000000000 ) ) ;
#7045 = DIRECTION ( 'NONE',  ( -0.9925485533564399887, 0.000000000000000000, 0.1218497814115315075 ) ) ;
#7046 = EDGE_CURVE ( 'NONE', #1701, #7088, #4535, .T. ) ;
#7047 = EDGE_CURVE ( 'NONE', #1742, #1500, #73, .T. ) ;
#7048 = ORIENTED_EDGE ( 'NONE', *, *, #2084, .T. ) ;
#7049 = PLANE ( 'NONE',  #6854 ) ;
#7050 = EDGE_CURVE ( 'NONE', #5163, #1840, #6823, .T. ) ;
#7051 = CARTESIAN_POINT ( 'NONE',  ( -3.987046614173228587, 4.076635394620980790, 8.381772284349393587 ) ) ;
#7052 = ORIENTED_EDGE ( 'NONE', *, *, #7317, .T. ) ;
#7053 = CARTESIAN_POINT ( 'NONE',  ( -4.382879947506562068, 4.383999996532200960, 8.231249998505111520 ) ) ;
#7054 = DIRECTION ( 'NONE',  ( 0.9999998435093852001, 1.024278174869913598E-17, -0.0005594472316433852718 ) ) ;
#7055 = CARTESIAN_POINT ( 'NONE',  ( -1.187500000000000666, 4.350832443807077787, 6.674940516136684820 ) ) ;
#7056 = DIRECTION ( 'NONE',  ( -0.7071067811865474617, 0.000000000000000000, -0.7071067811865474617 ) ) ;
#7057 = PERSON_AND_ORGANIZATION ( #7862, #8117 ) ;
#7058 = VERTEX_POINT ( 'NONE', #2628 ) ;
#7059 = CARTESIAN_POINT ( 'NONE',  ( -4.462046614173229564, 4.146499994075099060, 8.624249954778562710 ) ) ;
#7060 = PRODUCT_DEFINITION_SHAPE ( 'NONE', 'NONE',  #8192 ) ;
#7061 =( CONVERSION_BASED_UNIT ( 'INCH', #864 ) LENGTH_UNIT ( ) NAMED_UNIT ( #3083 ) );
#7062 = CYLINDRICAL_SURFACE ( 'NONE', #5275, 0.3125000000000016653 ) ;
#7063 = PERSON_AND_ORGANIZATION ( #7862, #8117 ) ;
#7064 = ORIENTED_EDGE ( 'NONE', *, *, #3211, .T. ) ;
#7065 = CARTESIAN_POINT ( 'NONE',  ( -0.7122575715994516887, 3.714602561338662845, 8.024726960321794778 ) ) ;
#7066 = ORIENTED_EDGE ( 'NONE', *, *, #7755, .F. ) ;
#7067 = CARTESIAN_POINT ( 'NONE',  ( 3.987953385826774166, 3.974973691467368120, 8.034752674066883316 ) ) ;
#7068 = CARTESIAN_POINT ( 'NONE',  ( 3.343750000000002220, 2.500000000000000444, -0.5625000000000003331 ) ) ;
#7069 = CARTESIAN_POINT ( 'NONE',  ( 3.987953385826772390, 4.131461189140908985, 8.306660907471565380 ) ) ;
#7070 = CARTESIAN_POINT ( 'NONE',  ( -0.6956352003900578840, 3.669529528902300441, 8.370551401437294814 ) ) ;
#7071 =( BOUNDED_SURFACE ( )  B_SPLINE_SURFACE ( 3, 3, ( 
 ( #8165, #4159, #4199, #4865 ),
 ( #1757, #2334, #6683, #3556 ),
 ( #2497, #6715, #4907, #8124 ),
 ( #1102, #3645, #4828, #6057 ),
 ( #6142, #2464, #4984, #4409 ),
 ( #6914, #5725, #3901, #5181 ) ),
 .UNSPECIFIED., .F., .F., .F. ) 
 B_SPLINE_SURFACE_WITH_KNOTS ( ( 4, 2, 4 ),
 ( 4, 4 ),
 ( 0.000000000000000000, 0.5000000000000000000, 1.000000000000000000 ),
 ( 0.000000000000000000, 1.000000000000000000 ),
 .UNSPECIFIED. ) 
 GEOMETRIC_REPRESENTATION_ITEM ( )  RATIONAL_B_SPLINE_SURFACE ( (
 ( 1.000000000000000000, 0.3333333333333332038, 0.3333333333333332038, 1.000000000000000000),
 ( 1.000000000000000000, 0.3333333333333332038, 0.3333333333333332038, 1.000000000000000000),
 ( 1.000000000000000000, 0.3333333333333332038, 0.3333333333333332038, 1.000000000000000000),
 ( 1.000000000000000000, 0.3333333333333332038, 0.3333333333333332038, 1.000000000000000000),
 ( 1.000000000000000000, 0.3333333333333332038, 0.3333333333333332038, 1.000000000000000000),
 ( 1.000000000000000000, 0.3333333333333332038, 0.3333333333333332038, 1.000000000000000000) ) ) 
 REPRESENTATION_ITEM ( '' )  SURFACE ( )  );
#7072 = ORIENTED_EDGE ( 'NONE', *, *, #3526, .F. ) ;
#7073 = CC_DESIGN_PERSON_AND_ORGANIZATION_ASSIGNMENT ( #7604, #2611, ( #1579 ) ) ;
#7074 = APPROVAL_PERSON_ORGANIZATION ( #4149, #6072, #976 ) ;
#7075 = DIRECTION ( 'NONE',  ( 0.000000000000000000, 0.000000000000000000, 1.000000000000000000 ) ) ;
#7076 = DIRECTION ( 'NONE',  ( 0.000000000000000000, 0.000000000000000000, -1.000000000000000000 ) ) ;
#7077 = ORIENTED_EDGE ( 'NONE', *, *, #1200, .F. ) ;
#7078 = APPROVAL_PERSON_ORGANIZATION ( #3604, #7968, #5352 ) ;
#7079 = APPROVAL_DATE_TIME ( #4529, #4518 ) ;
#7080 = FACE_OUTER_BOUND ( 'NONE', #6330, .T. ) ;
#7081 = CALENDAR_DATE ( 2026, 8, 10 ) ;
#7082 = CARTESIAN_POINT ( 'NONE',  ( 0.7499999999999993339, 3.950000000000000178, 7.918749999999998401 ) ) ;
#7083 = LINE ( 'NONE', #7766, #4404 ) ;
#7084 = APPROVAL ( #5556, 'UNSPECIFIED' ) ;
#7085 = EDGE_LOOP ( 'NONE', ( #3151, #3729, #732, #3686 ) ) ;
#7086 = DIRECTION ( 'NONE',  ( 1.000000000000000000, 1.681137226870316085E-15, 0.000000000000000000 ) ) ;
#7087 = CARTESIAN_POINT ( 'NONE',  ( -3.987046614173228587, 3.882766440201689484, 8.415903052206909152 ) ) ;
#7088 = VERTEX_POINT ( 'NONE', #6906 ) ;
#7089 = FACE_OUTER_BOUND ( 'NONE', #5426, .T. ) ;
#7090 = DIRECTION ( 'NONE',  ( 1.000000000000000000, 0.000000000000000000, 0.000000000000000000 ) ) ;
#7091 = CARTESIAN_POINT ( 'NONE',  ( 2.750000000000000444, 7.339000000000001300, 4.486250000000000959 ) ) ;
#7092 = DIRECTION ( 'NONE',  ( 0.5773502691896257311, -0.5773502691896257311, -0.5773502691896257311 ) ) ;
#7093 = EDGE_CURVE ( 'NONE', #2271, #6766, #1329, .T. ) ;
#7094 = APPROVAL_DATE_TIME ( #5194, #2908 ) ;
#7095 = ORIENTED_EDGE ( 'NONE', *, *, #4625, .T. ) ;
#7096 = EDGE_CURVE ( 'NONE', #4179, #4253, #4399, .T. ) ;
#7097 = CARTESIAN_POINT ( 'NONE',  ( -1.246236536363908742, 3.529356956552051283, -5.108750000000002345 ) ) ;
#7098 = CARTESIAN_POINT ( 'NONE',  ( 4.462953385826772923, 3.753500037801648759, 8.624249954778562710 ) ) ;
#7099 = CARTESIAN_POINT ( 'NONE',  ( -2.750000000000000444, 7.964000000000000412, 2.411250000000000338 ) ) ;
#7100 = LENGTH_MEASURE_WITH_UNIT ( LENGTH_MEASURE( 0.02539999999999999897 ), #7784 );
#7101 = DIRECTION ( 'NONE',  ( -0.000000000000000000, -1.000000000000000000, -0.000000000000000000 ) ) ;
#7102 = VERTEX_POINT ( 'NONE', #6414 ) ;
#7103 = PERSON_AND_ORGANIZATION_ROLE ( 'creator' ) ;
#7104 = ORIENTED_EDGE ( 'NONE', *, *, #4851, .T. ) ;
#7105 = CARTESIAN_POINT ( 'NONE',  ( -0.6836440906233618442, 3.641559347637748356, 8.180003846963320058 ) ) ;
#7106 = DESIGN_CONTEXT ( 'detailed design', #7415, 'design' ) ;
#7107 = B_SPLINE_CURVE_WITH_KNOTS ( 'NONE', 3,
 ( #6632, #5587, #5658, #37, #1201, #4850, #633, #1165, #2516, #4359, #1737, #4275 ),
 .UNSPECIFIED., .F., .F.,
 ( 4, 2, 2, 2, 2, 4 ),
 ( -0.01980159854141738326, -0.01485119890606303311, -0.009900799270708686428, -0.007425599453031514821, -0.004950399635354338010, 1.040834085586084257E-17 ),
 .UNSPECIFIED. ) ;
#7108 = CARTESIAN_POINT ( 'NONE',  ( 3.987953385826772390, 3.878440408003577922, 8.048241480259036962 ) ) ;
#7109 = ADVANCED_FACE ( 'NONE', ( #1294 ), #6861, .F. ) ;
#7110 = LINE ( 'NONE', #5326, #970 ) ;
#7111 = FACE_OUTER_BOUND ( 'NONE', #6541, .T. ) ;
#7112 = PERSON ( 'NAUO-PER9', 'UNSPECIFIED', 'UNSPECIFIED', ('UNSPECIFIED'), ('UNSPECIFIED'), ('UNSPECIFIED') ) ;
#7113 = VERTEX_POINT ( 'NONE', #3746 ) ;
#7114 = CARTESIAN_POINT ( 'NONE',  ( 3.987953385826771946, 4.135047251020852244, 8.297661934733794098 ) ) ;
#7115 = ORIENTED_EDGE ( 'NONE', *, *, #5767, .T. ) ;
#7116 = VECTOR ( 'NONE', #1130, 39.37007874015748854 ) ;
#7117 = CC_DESIGN_APPROVAL ( #5621, ( #4922 ) ) ;
#7118 = PLANE ( 'NONE',  #3069 ) ;
#7119 = ORIENTED_EDGE ( 'NONE', *, *, #2792, .F. ) ;
#7120 = APPROVAL_STATUS ( 'not_yet_approved' ) ;
#7121 = AXIS2_PLACEMENT_3D ( 'NONE', #2106, #7712, #2065 ) ;
#7122 = FACE_OUTER_BOUND ( 'NONE', #7654, .T. ) ;
#7123 = CALENDAR_DATE ( 2026, 8, 10 ) ;
#7124 = CARTESIAN_POINT ( 'NONE',  ( 2.750000000000000444, 8.601289606299213020, 3.691250000000001030 ) ) ;
#7125 = VECTOR ( 'NONE', #2320, 39.37007874015748143 ) ;
#7126 = ORIENTED_EDGE ( 'NONE', *, *, #2383, .T. ) ;
#7127 = CARTESIAN_POINT ( 'NONE',  ( -3.987046614173228143, 3.789313681612213713, 8.344403569825507461 ) ) ;
#7128 = ORIENTED_EDGE ( 'NONE', *, *, #5433, .F. ) ;
#7129 = FACE_OUTER_BOUND ( 'NONE', #3025, .T. ) ;
#7130 = CARTESIAN_POINT ( 'NONE',  ( 1.406273820872161684, 2.812660052342375927, 7.277379520629159160 ) ) ;
#7131 = APPROVAL ( #3704, 'UNSPECIFIED' ) ;
#7132 = DIRECTION ( 'NONE',  ( -0.000000000000000000, -1.000000000000000000, -0.000000000000000000 ) ) ;
#7133 = VECTOR ( 'NONE', #7622, 39.37007874015748143 ) ;
#7134 = CARTESIAN_POINT ( 'NONE',  ( -8.751021560936518753E-10, 1.000000000000000222, 3.874999999600099443 ) ) ;
#7135 = COORDINATED_UNIVERSAL_TIME_OFFSET ( 0, 0, .AHEAD. ) ;
#7136 = VERTEX_POINT ( 'NONE', #5665 ) ;
#7137 = VECTOR ( 'NONE', #230, 39.37007874015748143 ) ;
#7138 = CARTESIAN_POINT ( 'NONE',  ( -0.4244989081355610150, 2.705063376247227591, -5.108750000000003233 ) ) ;
#7139 = LOCAL_TIME ( 0, 37, 23.00000000000000000, #4866 ) ;
#7140 = DIRECTION ( 'NONE',  ( -0.5773502691896258421, -0.5773502691896258421, -0.5773502691896258421 ) ) ;
#7141 = ADVANCED_FACE ( 'NONE', ( #5129 ), #3894, .F. ) ;
#7142 = CYLINDRICAL_SURFACE ( 'NONE', #7688, 0.3625000012227142521 ) ;
#7143 = ORIENTED_EDGE ( 'NONE', *, *, #4224, .T. ) ;
#7144 = PERSON_AND_ORGANIZATION ( #7862, #8117 ) ;
#7145 = ORIENTED_EDGE ( 'NONE', *, *, #4265, .F. ) ;
#7146 = CARTESIAN_POINT ( 'NONE',  ( -0.7253895767696343366, 3.758660869344151223, 7.983341084825773315 ) ) ;
#7147 = CARTESIAN_POINT ( 'NONE',  ( 0.6836440906233619552, 3.641559347637747912, 8.282496153036683850 ) ) ;
#7148 = EDGE_CURVE ( 'NONE', #5130, #2954, #6329, .T. ) ;
#7149 = VECTOR ( 'NONE', #7164, 39.37007874015748143 ) ;
#7150 = DIRECTION ( 'NONE',  ( -0.000000000000000000, 1.000000000000000000, -0.000000000000000000 ) ) ;
#7151 = VECTOR ( 'NONE', #3985, 39.37007874015748143 ) ;
#7152 = CARTESIAN_POINT ( 'NONE',  ( 0.000000000000000000, 2.762500000000000178, 6.956250000000000711 ) ) ;
#7153 = EDGE_CURVE ( 'NONE', #963, #6736, #757, .T. ) ;
#7154 = CARTESIAN_POINT ( 'NONE',  ( 3.987953385826771946, 4.001800847919377624, 8.420997134034163167 ) ) ;
#7155 = ORIENTED_EDGE ( 'NONE', *, *, #4966, .T. ) ;
#7156 = AXIS2_PLACEMENT_3D ( 'NONE', #3189, #1343, #7086 ) ;
#7157 = EDGE_CURVE ( 'NONE', #4596, #277, #3212, .T. ) ;
#7158 = CARTESIAN_POINT ( 'NONE',  ( 0.000000000000000000, 3.950000000000000178, 7.231250000000000178 ) ) ;
#7159 = EDGE_CURVE ( 'NONE', #4502, #1993, #2188, .T. ) ;
#7160 = VECTOR ( 'NONE', #4974, 39.37007874015748854 ) ;
#7161 = LINE ( 'NONE', #4064, #2022 ) ;
#7162 = CIRCLE ( 'NONE', #7035, 0.1875000000000006661 ) ;
#7163 = DATE_TIME_ROLE ( 'classification_date' ) ;
#7164 = DIRECTION ( 'NONE',  ( -0.000000000000000000, 1.000000000000000000, 0.000000000000000000 ) ) ;
#7165 = COORDINATED_UNIVERSAL_TIME_OFFSET ( 0, 0, .AHEAD. ) ;
#7166 = DIRECTION ( 'NONE',  ( 0.000000000000000000, 0.000000000000000000, -1.000000000000000000 ) ) ;
#7167 = EDGE_CURVE ( 'NONE', #5899, #2271, #5000, .T. ) ;
#7168 = VECTOR ( 'NONE', #418, 39.37007874015748143 ) ;
#7169 = EDGE_LOOP ( 'NONE', ( #7632, #3355, #2120, #6328 ) ) ;
#7170 = PLANE ( 'NONE',  #5047 ) ;
#7171 = CARTESIAN_POINT ( 'NONE',  ( -3.987046614173228587, 4.130262297440223662, 8.309748556456774793 ) ) ;
#7172 = FACE_OUTER_BOUND ( 'NONE', #1988, .T. ) ;
#7173 = DIRECTION ( 'NONE',  ( 0.000000000000000000, 1.000000000000000000, 0.000000000000000000 ) ) ;
#7174 = ORIENTED_EDGE ( 'NONE', *, *, #7004, .T. ) ;
#7175 = DIRECTION ( 'NONE',  ( 0.9999998435093852001, -2.632258801812469973E-16, -0.0005594472316432187384 ) ) ;
#7176 = PLANE ( 'NONE',  #328 ) ;
#7177 = PERSON_AND_ORGANIZATION ( #7862, #8117 ) ;
#7178 = EDGE_LOOP ( 'NONE', ( #3204, #6677 ) ) ;
#7179 = CARTESIAN_POINT ( 'NONE',  ( 2.537499998660271761, 3.550000000000001155, 2.790532913385826763 ) ) ;
#7180 = CC_DESIGN_PERSON_AND_ORGANIZATION_ASSIGNMENT ( #7177, #286, ( #8153 ) ) ;
#7181 = CARTESIAN_POINT ( 'NONE',  ( -1.196592970772699660, 3.410287616584806170, -5.108749999999999680 ) ) ;
#7182 = CARTESIAN_POINT ( 'NONE',  ( 0.01493480814038263167, 2.324986238204167943, 3.080221901019060127 ) ) ;
#7183 = PLANE ( 'NONE',  #1888 ) ;
#7184 = CC_DESIGN_APPROVAL ( #6638, ( #1319 ) ) ;
#7185 = CARTESIAN_POINT ( 'NONE',  ( 2.750000000000000444, 8.729000000000002757, 4.313750000000002416 ) ) ;
#7186 = EDGE_CURVE ( 'NONE', #6458, #4928, #1207, .T. ) ;
#7187 = APPLICATION_PROTOCOL_DEFINITION ( 'international standard', 'config_control_design', 1994, #6081 ) ;
#7188 = EDGE_LOOP ( 'NONE', ( #7881, #7596, #4537 ) ) ;
#7189 = CARTESIAN_POINT ( 'NONE',  ( -0.7370170160409605931, 3.810752038529027885, 7.951302674248323932 ) ) ;
#7190 = APPROVAL ( #2333, 'UNSPECIFIED' ) ;
#7191 = PLANE ( 'NONE',  #2538 ) ;
#7192 = CARTESIAN_POINT ( 'NONE',  ( 0.000000000000000000, 2.359000000000000874, 3.956250000000000266 ) ) ;
#7193 = CARTESIAN_POINT ( 'NONE',  ( 3.874999998766638587, 1.000000000000000222, -3.894564048797845777E-16 ) ) ;
#7194 = MANIFOLD_SOLID_BREP ( 'Imported1', #2162 ) ;
#7195 = CARTESIAN_POINT ( 'NONE',  ( 3.987953385826771946, 4.021559623872877687, 8.414258516751351280 ) ) ;
#7196 = EDGE_CURVE ( 'NONE', #6895, #5506, #2591, .T. ) ;
#7197 = EDGE_CURVE ( 'NONE', #2439, #7750, #340, .T. ) ;
#7198 = ORIENTED_EDGE ( 'NONE', *, *, #4052, .F. ) ;
#7199 = EDGE_CURVE ( 'NONE', #5688, #1328, #2228, .T. ) ;
#7200 = CARTESIAN_POINT ( 'NONE',  ( -3.987046614173228587, 3.950000015938371689, 7.918750010554200358 ) ) ;
#7201 = CARTESIAN_POINT ( 'NONE',  ( -2.750000000000000444, 7.521783346469146814, 3.956249999992520916 ) ) ;
#7202 = CARTESIAN_POINT ( 'NONE',  ( -2.750000000000000888, 7.964000000000000412, 3.813750000000002416 ) ) ;
#7203 = CARTESIAN_POINT ( 'NONE',  ( 0.000000000000000000, 2.661265787401576155, 3.956250000000001155 ) ) ;
#7204 = CARTESIAN_POINT ( 'NONE',  ( 2.740000000000000213, 8.729000000000002757, 3.823750000000002647 ) ) ;
#7205 = APPROVAL_STATUS ( 'not_yet_approved' ) ;
#7206 = DIRECTION ( 'NONE',  ( 0.000000000000000000, 0.000000000000000000, -1.000000000000000000 ) ) ;
#7207 = APPROVAL_ROLE ( '' ) ;
#7208 = CARTESIAN_POINT ( 'NONE',  ( 0.6854931847115989241, 4.254309166866921288, 8.303072425453407845 ) ) ;
#7209 = PLANE ( 'NONE',  #4801 ) ;
#7210 = ORIENTED_EDGE ( 'NONE', *, *, #5828, .F. ) ;
#7211 = LINE ( 'NONE', #5428, #4526 ) ;
#7212 = CC_DESIGN_SECURITY_CLASSIFICATION ( #5099, ( #8189 ) ) ;
#7213 = ORIENTED_EDGE ( 'NONE', *, *, #5601, .F. ) ;
#7214 = CARTESIAN_POINT ( 'NONE',  ( -2.150000000000000799, 2.875000000000001332, 3.742515787401574645 ) ) ;
#7215 = VERTEX_POINT ( 'NONE', #832 ) ;
#7216 = APPLICATION_PROTOCOL_DEFINITION ( 'international standard', 'config_control_design', 1994, #2730 ) ;
#7217 = DIRECTION ( 'NONE',  ( 1.000000000000000000, -0.000000000000000000, 0.000000000000000000 ) ) ;
#7218 = PERSON_AND_ORGANIZATION_ROLE ( 'design_owner' ) ;
#7219 = ADVANCED_BREP_SHAPE_REPRESENTATION ( '', ( #1772, #7272 ), #5419 ) ;
#7220 = EDGE_LOOP ( 'NONE', ( #335, #6639 ) ) ;
#7221 = LOCAL_TIME ( 0, 37, 23.00000000000000000, #4795 ) ;
#7222 = CARTESIAN_POINT ( 'NONE',  ( -0.8670766215445633307, 2.963758944386602590, -5.108749999999997904 ) ) ;
#7223 = CARTESIAN_POINT ( 'NONE',  ( 0.6796442504223291214, 2.472718385001931196, 2.935424685056315486 ) ) ;
#7224 = CARTESIAN_POINT ( 'NONE',  ( 4.470366332363715500, 1.365923996832131609E-16, 2.937534001674282358 ) ) ;
#7225 =( NAMED_UNIT ( * ) SI_UNIT ( $, .STERADIAN. ) SOLID_ANGLE_UNIT ( ) );
#7226 = CARTESIAN_POINT ( 'NONE',  ( 3.762484563843161212, 1.281112611882646579, 0.000000000000000000 ) ) ;
#7227 = APPROVAL_ROLE ( '' ) ;
#7228 = EDGE_LOOP ( 'NONE', ( #5467, #6506, #6678, #7095, #6802, #4694 ) ) ;
#7229 = CARTESIAN_POINT ( 'NONE',  ( -3.583510604133041344, 1.543025754838327046, 4.388534791062126923E-16 ) ) ;
#7230 = ADVANCED_FACE ( 'NONE', ( #3337 ), #4719, .T. ) ;
#7231 = PERSON ( 'NAUO-PER2', 'UNSPECIFIED', 'UNSPECIFIED', ('UNSPECIFIED'), ('UNSPECIFIED'), ('UNSPECIFIED') ) ;
#7232 = DIRECTION ( 'NONE',  ( 0.000000000000000000, -0.000000000000000000, -1.000000000000000000 ) ) ;
#7233 = CARTESIAN_POINT ( 'NONE',  ( 4.462953385826773811, 3.674333370316265501, 7.679916707260901809 ) ) ;
#7234 = DIRECTION ( 'NONE',  ( 0.000000000000000000, 0.000000000000000000, -1.000000000000000000 ) ) ;
#7235 = ORIENTED_EDGE ( 'NONE', *, *, #4583, .T. ) ;
#7236 = CC_DESIGN_DATE_AND_TIME_ASSIGNMENT ( #4770, #7339, ( #7978 ) ) ;
#7237 = CARTESIAN_POINT ( 'NONE',  ( 2.537499998660271761, 3.550000000000001155, -1.169467086614173645 ) ) ;
#7238 = VERTEX_POINT ( 'NONE', #7756 ) ;
#7239 = EDGE_CURVE ( 'NONE', #7672, #2992, #4601, .T. ) ;
#7240 = DIRECTION ( 'NONE',  ( 0.000000000000000000, -0.000000000000000000, 1.000000000000000000 ) ) ;
#7241 = CARTESIAN_POINT ( 'NONE',  ( -1.624999999999998446, 3.950000000000000178, 2.749999998413802160 ) ) ;
#7242 = FACE_OUTER_BOUND ( 'NONE', #4990, .T. ) ;
#7243 = DIRECTION ( 'NONE',  ( -1.000000000000000000, 0.000000000000000000, 0.000000000000000000 ) ) ;
#7244 = VERTEX_POINT ( 'NONE', #3376 ) ;
#7245 = CALENDAR_DATE ( 2026, 8, 10 ) ;
#7246 = DIRECTION ( 'NONE',  ( -0.000000000000000000, 1.000000000000000000, -0.000000000000000000 ) ) ;
#7247 = CARTESIAN_POINT ( 'NONE',  ( 0.6892550738286248313, 4.245699673162182108, 8.332856313163132356 ) ) ;
#7248 = PLANE ( 'NONE',  #7855 ) ;
#7249 = SECURITY_CLASSIFICATION ( '', '', #5018 ) ;
#7250 = CARTESIAN_POINT ( 'NONE',  ( 0.000000000000000000, 5.536672282146935409, 4.083473622047245399 ) ) ;
#7251 = MANIFOLD_SOLID_BREP ( 'Imported1', #5289 ) ;
#7252 = ORIENTED_EDGE ( 'NONE', *, *, #3268, .F. ) ;
#7253 = CARTESIAN_POINT ( 'NONE',  ( -3.182000000000000828, 2.359000000000000874, 3.956250000000000266 ) ) ;
#7254 = VECTOR ( 'NONE', #5363, 39.37007874015748854 ) ;
#7255 = CC_DESIGN_APPROVAL ( #3264, ( #3521 ) ) ;
#7256 = VERTEX_POINT ( 'NONE', #265 ) ;
#7257 = LINE ( 'NONE', #898, #3463 ) ;
#7258 = ORIENTED_EDGE ( 'NONE', *, *, #1919, .T. ) ;
#7259 = DATE_AND_TIME ( #1063, #1870 ) ;
#7260 = DIRECTION ( 'NONE',  ( -0.000000000000000000, 1.000000000000000000, 0.000000000000000000 ) ) ;
#7261 = DATE_AND_TIME ( #1720, #1315 ) ;
#7262 = VERTEX_POINT ( 'NONE', #2760 ) ;
#7263 = CARTESIAN_POINT ( 'NONE',  ( -1.624999999371729231, 2.076218724780642511, 2.750000000000000444 ) ) ;
#7264 = AXIS2_PLACEMENT_3D ( 'NONE', #2764, #5249, #510 ) ;
#7265 = AXIS2_PLACEMENT_3D ( 'NONE', #6243, #4931, #7470 ) ;
#7266 = CARTESIAN_POINT ( 'NONE',  ( 0.000000000000000000, 1.664000000000000368, 2.693920355039552791E-42 ) ) ;
#7267 = CARTESIAN_POINT ( 'NONE',  ( -0.2597574076448537772, 2.345571136547101254, 3.059942488945281536 ) ) ;
#7268 = AXIS2_PLACEMENT_3D ( 'NONE', #5160, #7706, #704 ) ;
#7269 = DIRECTION ( 'NONE',  ( 0.000000000000000000, 0.000000000000000000, 1.000000000000000000 ) ) ;
#7270 = VECTOR ( 'NONE', #6109, 39.37007874015748143 ) ;
#7271 = DIRECTION ( 'NONE',  ( 0.000000000000000000, 0.000000000000000000, -1.000000000000000000 ) ) ;
#7272 = AXIS2_PLACEMENT_3D ( 'NONE', #3736, #6237, #5618 ) ;
#7273 = MECHANICAL_CONTEXT ( 'NONE', #6081, 'mechanical' ) ;
#7274 = EDGE_LOOP ( 'NONE', ( #8136, #1675 ) ) ;
#7275 = CARTESIAN_POINT ( 'NONE',  ( 2.750000000000000444, 8.719000000000002970, 3.823750000000002647 ) ) ;
#7276 = CIRCLE ( 'NONE', #6864, 3.874999999025058095 ) ;
#7277 = EDGE_CURVE ( 'NONE', #7866, #5331, #5245, .T. ) ;
#7278 = LOCAL_TIME ( 0, 37, 23.00000000000000000, #8166 ) ;
#7279 = CARTESIAN_POINT ( 'NONE',  ( 0.7335700393700786970, 2.500000000000000444, 2.909883779527559611 ) ) ;
#7280 = DIRECTION ( 'NONE',  ( 0.000000000000000000, 1.000000000000000000, 0.000000000000000000 ) ) ;
#7281 = CARTESIAN_POINT ( 'NONE',  ( -3.562500000000000444, 1.000000000000000222, 2.975000000000000977 ) ) ;
#7282 = CARTESIAN_POINT ( 'NONE',  ( -2.750000000000000444, 7.964000000000000412, 4.323750000000003091 ) ) ;
#7283 = CARTESIAN_POINT ( 'NONE',  ( -2.875000000000000888, -3.820994292482255198E-18, -2.975000000000000977 ) ) ;
#7284 = LOCAL_TIME ( 0, 37, 23.00000000000000000, #6303 ) ;
#7285 = DIRECTION ( 'NONE',  ( 0.000000000000000000, 0.000000000000000000, -1.000000000000000000 ) ) ;
#7286 = CARTESIAN_POINT ( 'NONE',  ( -0.6820189411826723669, 3.637988102632602416, 8.210925237484662631 ) ) ;
#7287 = ORIENTED_EDGE ( 'NONE', *, *, #333, .T. ) ;
#7288 = VECTOR ( 'NONE', #599, 39.37007874015748143 ) ;
#7289 = VECTOR ( 'NONE', #7980, 39.37007874015748143 ) ;
#7290 = CC_DESIGN_PERSON_AND_ORGANIZATION_ASSIGNMENT ( #4702, #5818, ( #1164 ) ) ;
#7291 = PRODUCT_DEFINITION_FORMATION_WITH_SPECIFIED_SOURCE ( 'ANY', '', #2360, .NOT_KNOWN. ) ;
#7292 = CARTESIAN_POINT ( 'NONE',  ( -3.987046614173227699, 4.142138515950292366, 8.190024801382838504 ) ) ;
#7293 = DIRECTION ( 'NONE',  ( -0.000000000000000000, 1.000000000000000000, -0.000000000000000000 ) ) ;
#7294 = CARTESIAN_POINT ( 'NONE',  ( 0.5069887433553049716, 2.405790110920277503, -3.000813131718135462 ) ) ;
#7295 = CARTESIAN_POINT ( 'NONE',  ( 2.740000000000000657, 7.974000000000001087, 3.323750000000001759 ) ) ;
#7296 = CARTESIAN_POINT ( 'NONE',  ( -1.625000000000000222, 5.639000000000001123, 0.000000000000000000 ) ) ;
#7297 = VERTEX_POINT ( 'NONE', #5455 ) ;
#7298 = ADVANCED_FACE ( 'NONE', ( #7974 ), #1782, .F. ) ;
#7299 = CALENDAR_DATE ( 2026, 8, 10 ) ;
#7300 = DIRECTION ( 'NONE',  ( 0.000000000000000000, 0.000000000000000000, 1.000000000000000000 ) ) ;
#7301 = CIRCLE ( 'NONE', #1128, 3.874999999025058095 ) ;
#7302 = CONTEXT_DEPENDENT_SHAPE_REPRESENTATION ( #6565, #6987 ) ;
#7303 = CARTESIAN_POINT ( 'NONE',  ( 0.7386972477860228592, 4.080064161770346587, 7.946921043053440492 ) ) ;
#7304 = DIRECTION ( 'NONE',  ( -0.000000000000000000, 0.7071067811865474617, -0.7071067811865474617 ) ) ;
#7305 = EDGE_LOOP ( 'NONE', ( #7001, #1850 ) ) ;
#7306 = PLANE ( 'NONE',  #2055 ) ;
#7307 = ORIENTED_EDGE ( 'NONE', *, *, #1798, .F. ) ;
#7308 = DIRECTION ( 'NONE',  ( 0.000000000000000000, 1.000000000000000000, 0.000000000000000000 ) ) ;
#7309 = DIRECTION ( 'NONE',  ( -0.000000000000000000, 0.000000000000000000, -1.000000000000000000 ) ) ;
#7310 = ORIENTED_EDGE ( 'NONE', *, *, #4040, .T. ) ;
#7311 = COORDINATED_UNIVERSAL_TIME_OFFSET ( 0, 0, .AHEAD. ) ;
#7312 = DIRECTION ( 'NONE',  ( -0.000000000000000000, -1.000000000000000000, -0.000000000000000000 ) ) ;
#7313 = LINE ( 'NONE', #7775, #6486 ) ;
#7314 = EDGE_CURVE ( 'NONE', #6365, #4981, #2262, .T. ) ;
#7315 = APPROVAL_DATE_TIME ( #2290, #6214 ) ;
#7316 = ORIENTED_EDGE ( 'NONE', *, *, #1426, .F. ) ;
#7317 = EDGE_CURVE ( 'NONE', #2772, #5647, #2312, .T. ) ;
#7318 = AXIS2_PLACEMENT_3D ( 'NONE', #4729, #978, #238 ) ;
#7319 = VECTOR ( 'NONE', #500, 39.37007874015748143 ) ;
#7320 = EDGE_CURVE ( 'NONE', #6945, #2985, #4180, .T. ) ;
#7321 = CARTESIAN_POINT ( 'NONE',  ( -2.740000000000001545, 8.724000000000001975, 3.828750000000002096 ) ) ;
#7322 = CARTESIAN_POINT ( 'NONE',  ( -0.7078558382242214897, 4.198166876146032678, 8.040237954860636194 ) ) ;
#7323 = CARTESIAN_POINT ( 'NONE',  ( 3.762484563843161656, 1.281112611882646579, 7.524969127686321535 ) ) ;
#7324 = CALENDAR_DATE ( 2026, 8, 10 ) ;
#7325 = EDGE_LOOP ( 'NONE', ( #2637, #7052, #7458, #4365 ) ) ;
#7326 = CARTESIAN_POINT ( 'NONE',  ( -3.362500000000001155, 1.750000000000000444, 4.117874862132976456E-16 ) ) ;
#7327 = LOCAL_TIME ( 0, 37, 23.00000000000000000, #4872 ) ;
#7328 = CARTESIAN_POINT ( 'NONE',  ( 0.000000000000000000, 5.160877715062512472, 6.858307716807694909 ) ) ;
#7329 = PLANE ( 'NONE',  #7677 ) ;
#7330 = ORIENTED_EDGE ( 'NONE', *, *, #7444, .F. ) ;
#7331 = CARTESIAN_POINT ( 'NONE',  ( -3.791570908345035740, 1.365923996832131609E-16, 0.7997593681799630705 ) ) ;
#7332 = ORIENTED_EDGE ( 'NONE', *, *, #4329, .T. ) ;
#7333 = CC_DESIGN_APPROVAL ( #1365, ( #6586 ) ) ;
#7334 = CARTESIAN_POINT ( 'NONE',  ( -3.987046614173228587, 4.146499994074616779, 8.231249998505111520 ) ) ;
#7335 = DIRECTION ( 'NONE',  ( 0.000000000000000000, -1.000000000000000000, 0.000000000000000000 ) ) ;
#7336 = CARTESIAN_POINT ( 'NONE',  ( 1.024630039370079126, 4.279065905511812318, -7.087001889763783424 ) ) ;
#7337 = FACE_OUTER_BOUND ( 'NONE', #3799, .T. ) ;
#7338 = VERTEX_POINT ( 'NONE', #7924 ) ;
#7339 = DATE_TIME_ROLE ( 'creation_date' ) ;
#7340 = FACE_OUTER_BOUND ( 'NONE', #5798, .T. ) ;
#7341 = DIRECTION ( 'NONE',  ( 0.000000000000000000, -0.000000000000000000, 1.000000000000000000 ) ) ;
#7342 = ORIENTED_EDGE ( 'NONE', *, *, #1336, .T. ) ;
#7343 = PLANE ( 'NONE',  #2839 ) ;
#7344 = FACE_OUTER_BOUND ( 'NONE', #3824, .T. ) ;
#7345 = DIRECTION ( 'NONE',  ( 0.000000000000000000, 0.000000000000000000, 1.000000000000000000 ) ) ;
#7346 = DIRECTION ( 'NONE',  ( 0.000000000000000000, 0.000000000000000000, -1.000000000000000000 ) ) ;
#7347 = ORIENTED_EDGE ( 'NONE', *, *, #2488, .T. ) ;
#7348 = COORDINATED_UNIVERSAL_TIME_OFFSET ( 0, 0, .AHEAD. ) ;
#7349 = DIRECTION ( 'NONE',  ( 0.000000000000000000, -0.7071067811865474617, 0.7071067811865474617 ) ) ;
#7350 = DATE_AND_TIME ( #1104, #6293 ) ;
#7351 = ORIENTED_EDGE ( 'NONE', *, *, #3644, .F. ) ;
#7352 = CC_DESIGN_PERSON_AND_ORGANIZATION_ASSIGNMENT ( #3055, #3222, ( #4741 ) ) ;
#7353 = DIRECTION ( 'NONE',  ( 1.000000000000000000, 0.000000000000000000, -0.000000000000000000 ) ) ;
#7354 = PRODUCT_DEFINITION_SHAPE ( 'NONE', 'NONE',  #1030 ) ;
#7355 = SHAPE_REPRESENTATION ( 'bench vise10-', ( #7272 ), #456 ) ;
#7356 = LOCAL_TIME ( 0, 37, 23.00000000000000000, #1180 ) ;
#7357 = CARTESIAN_POINT ( 'NONE',  ( -1.312500000000000444, 4.908106850393701315, 3.316250000000001474 ) ) ;
#7358 = CARTESIAN_POINT ( 'NONE',  ( -0.7417920657368231030, 4.061067302434975268, 7.938974592032496780 ) ) ;
#7359 = CARTESIAN_POINT ( 'NONE',  ( 0.000000000000000000, 1.750000000000000444, 0.000000000000000000 ) ) ;
#7360 = PERSON_AND_ORGANIZATION ( #7862, #8117 ) ;
#7361 = LOCAL_TIME ( 0, 37, 23.00000000000000000, #5400 ) ;
#7362 = ORIENTED_EDGE ( 'NONE', *, *, #62, .T. ) ;
#7363 = APPLICATION_CONTEXT ( 'configuration controlled 3d designs of mechanical parts and assemblies' ) ;
#7364 = EDGE_CURVE ( 'NONE', #6736, #5222, #6078, .T. ) ;
#7365 = CARTESIAN_POINT ( 'NONE',  ( 3.875000000000001776, 1.000000000000000222, -9.491012693391993703E-16 ) ) ;
#7366 = DIRECTION ( 'NONE',  ( 0.000000000000000000, 0.000000000000000000, 1.000000000000000000 ) ) ;
#7367 = LINE ( 'NONE', #6118, #7676 ) ;
#7368 = CARTESIAN_POINT ( 'NONE',  ( 2.750000000000000444, 8.574153540863029832, 4.323750000000001315 ) ) ;
#7369 = MANIFOLD_SOLID_BREP ( 'Imported1', #5690 ) ;
#7370 = EDGE_LOOP ( 'NONE', ( #1562, #1229, #5037, #2332 ) ) ;
#7371 = DIRECTION ( 'NONE',  ( 0.000000000000000000, 0.000000000000000000, 1.000000000000000000 ) ) ;
#7372 = ORIENTED_EDGE ( 'NONE', *, *, #2917, .T. ) ;
#7373 = EDGE_CURVE ( 'NONE', #3043, #6048, #3626, .T. ) ;
#7374 = EDGE_CURVE ( 'NONE', #5577, #6692, #384, .T. ) ;
#7375 = B_SPLINE_CURVE_WITH_KNOTS ( 'NONE', 3,
 ( #6521, #5255, #7813, #6385, #3904, #3941 ),
 .UNSPECIFIED., .F., .F.,
 ( 4, 2, 4 ),
 ( 0.000000000000000000, 0.007631658727031280162, 0.01526331745406256032 ),
 .UNSPECIFIED. ) ;
#7376 = LINE ( 'NONE', #6741, #7808 ) ;
#7377 = CARTESIAN_POINT ( 'NONE',  ( -0.9761938188976380104, 4.405876181102362565, -7.086507244094490510 ) ) ;
#7378 = CYLINDRICAL_SURFACE ( 'NONE', #7671, 0.4312500000000004663 ) ;
#7379 = CARTESIAN_POINT ( 'NONE',  ( -1.625000000000000222, 2.359134605132341189, -2.598586947523131574 ) ) ;
#7380 = EDGE_LOOP ( 'NONE', ( #6233, #6839 ) ) ;
#7381 = CALENDAR_DATE ( 2026, 8, 10 ) ;
#7382 = DIRECTION ( 'NONE',  ( 0.000000000000000000, 0.000000000000000000, 1.000000000000000000 ) ) ;
#7383 = COORDINATED_UNIVERSAL_TIME_OFFSET ( 0, 0, .AHEAD. ) ;
#7384 = EDGE_CURVE ( 'NONE', #6810, #2355, #6778, .T. ) ;
#7385 = VERTEX_POINT ( 'NONE', #1656 ) ;
#7386 = DIRECTION ( 'NONE',  ( 0.000000000000000000, 1.000000000000000000, 0.000000000000000000 ) ) ;
#7387 = CARTESIAN_POINT ( 'NONE',  ( -4.462046614173229564, 3.753500037802126599, 7.838250042232624004 ) ) ;
#7388 = CARTESIAN_POINT ( 'NONE',  ( -2.750000000000000888, 7.974000000000001087, 3.333750000000001990 ) ) ;
#7389 = EDGE_LOOP ( 'NONE', ( #2071, #4971, #1808, #4043 ) ) ;
#7390 = PERSON_AND_ORGANIZATION ( #7862, #8117 ) ;
#7391 = CARTESIAN_POINT ( 'NONE',  ( 4.476342532109287120, 3.950000015938371689, 8.231249998505111520 ) ) ;
#7392 = CARTESIAN_POINT ( 'NONE',  ( -0.7466433925744946354, 3.878406391858415514, 8.535611635381275875 ) ) ;
#7393 = CARTESIAN_POINT ( 'NONE',  ( -0.4206575637829014225, 5.194009207123433391, -5.108750000000004121 ) ) ;
#7394 = PERSON_AND_ORGANIZATION_ROLE ( 'classification_officer' ) ;
#7395 = VECTOR ( 'NONE', #5838, 39.37007874015748143 ) ;
#7396 = AXIS2_PLACEMENT_3D ( 'NONE', #7266, #1526, #5234 ) ;
#7397 = LOCAL_TIME ( 0, 37, 23.00000000000000000, #3900 ) ;
#7398 = CARTESIAN_POINT ( 'NONE',  ( -2.740000000000000213, 8.719000000000001194, 3.323750000000001759 ) ) ;
#7399 = DIRECTION ( 'NONE',  ( -3.865154999631033652E-14, 0.7071067811865474617, -0.7071067811865474617 ) ) ;
#7400 = CC_DESIGN_PERSON_AND_ORGANIZATION_ASSIGNMENT ( #3074, #3655, ( #6576 ) ) ;
#7401 = EDGE_LOOP ( 'NONE', ( #2745, #3544, #5749, #5410 ) ) ;
#7402 = CARTESIAN_POINT ( 'NONE',  ( -4.462046614173229564, 4.146499994074616779, 8.624249954777603477 ) ) ;
#7403 = CARTESIAN_POINT ( 'NONE',  ( 2.753607252840342579, 0.9999999999988802291, -2.731109880590252725 ) ) ;
#7404 = LINE ( 'NONE', #4257, #883 ) ;
#7405 = CALENDAR_DATE ( 2026, 8, 10 ) ;
#7406 = ORIENTED_EDGE ( 'NONE', *, *, #7910, .T. ) ;
#7407 = VECTOR ( 'NONE', #4312, 39.37007874015748143 ) ;
#7408 = DIRECTION ( 'NONE',  ( -0.000000000000000000, -1.000000000000000000, -0.000000000000000000 ) ) ;
#7409 = LOCAL_TIME ( 0, 37, 23.00000000000000000, #4896 ) ;
#7410 = VERTEX_POINT ( 'NONE', #6664 ) ;
#7411 = AXIS2_PLACEMENT_3D ( 'NONE', #3398, #7867, #6643 ) ;
#7412 = CC_DESIGN_PERSON_AND_ORGANIZATION_ASSIGNMENT ( #1025, #6681, ( #3944 ) ) ;
#7413 = CC_DESIGN_APPROVAL ( #6544, ( #7674 ) ) ;
#7414 = DIRECTION ( 'NONE',  ( -0.000000000000000000, 1.000000000000000000, -0.000000000000000000 ) ) ;
#7415 = APPLICATION_CONTEXT ( 'configuration controlled 3d designs of mechanical parts and assemblies' ) ;
#7416 = DIRECTION ( 'NONE',  ( 0.000000000000000000, -0.000000000000000000, 1.000000000000000000 ) ) ;
#7417 = CARTESIAN_POINT ( 'NONE',  ( 2.852014645669292303, 5.376007322834644775, 5.972081456692913015 ) ) ;
#7418 = EDGE_LOOP ( 'NONE', ( #4115, #1062, #478 ) ) ;
#7419 = LINE ( 'NONE', #7331, #3304 ) ;
#7420 = EDGE_CURVE ( 'NONE', #402, #4281, #5412, .T. ) ;
#7421 = EDGE_LOOP ( 'NONE', ( #436, #4826, #4884 ) ) ;
#7422 = AXIS2_PLACEMENT_3D ( 'NONE', #5580, #4844, #6695 ) ;
#7423 = ADVANCED_FACE ( 'NONE', ( #467 ), #6698, .T. ) ;
#7424 = EDGE_CURVE ( 'NONE', #3656, #7024, #820, .T. ) ;
#7425 = VECTOR ( 'NONE', #2172, 39.37007874015748143 ) ;
#7426 = CARTESIAN_POINT ( 'NONE',  ( 3.987953385826772390, 4.076635394618645769, 8.080727712659717454 ) ) ;
#7427 = CLOSED_SHELL ( 'NONE', ( #411, #5778, #686, #4285, #5939, #3346, #6931, #5537, #5743, #345, #5787, #1748, #1502, #327, #4940, #2129, #6579, #6334, #2387, #1447, #3983, #8158, #4721, #2441, #1674, #4025 ) ) ;
#7428 = CC_DESIGN_APPROVAL ( #3415, ( #5167 ) ) ;
#7429 = DIRECTION ( 'NONE',  ( -0.000000000000000000, -0.7071067811865474617, -0.7071067811865474617 ) ) ;
#7430 = DIRECTION ( 'NONE',  ( -1.000000000000000000, 0.000000000000000000, -0.000000000000000000 ) ) ;
#7431 = DIRECTION ( 'NONE',  ( 0.000000000000000000, 0.000000000000000000, -1.000000000000000000 ) ) ;
#7432 = EDGE_LOOP ( 'NONE', ( #283, #1691, #6615, #961 ) ) ;
#7433 = PERSON_AND_ORGANIZATION ( #7862, #8117 ) ;
#7434 = DIRECTION ( 'NONE',  ( 1.000000000000000000, 0.000000000000000000, -0.000000000000000000 ) ) ;
#7435 = ADVANCED_FACE ( 'NONE', ( #6121 ), #6737, .T. ) ;
#7436 = ORIENTED_EDGE ( 'NONE', *, *, #4927, .F. ) ;
#7437 = VECTOR ( 'NONE', #477, 39.37007874015748143 ) ;
#7438 = CARTESIAN_POINT ( 'NONE',  ( -3.987046614173228587, 4.225666661560477877, 8.231249998505111520 ) ) ;
#7439 = ORIENTED_EDGE ( 'NONE', *, *, #5493, .F. ) ;
#7440 = APPLICATION_PROTOCOL_DEFINITION ( 'international standard', 'config_control_design', 1994, #8182 ) ;
#7441 = CARTESIAN_POINT ( 'NONE',  ( -2.537500000000000533, 2.500000000000000444, 0.2625000000000008438 ) ) ;
#7442 = CALENDAR_DATE ( 2026, 8, 10 ) ;
#7443 = CARTESIAN_POINT ( 'NONE',  ( 3.362500000000000711, 1.750000000000000444, -4.117874862132976456E-16 ) ) ;
#7444 = EDGE_CURVE ( 'NONE', #4731, #6648, #6192, .T. ) ;
#7445 = DIRECTION ( 'NONE',  ( 0.000000000000000000, 0.000000000000000000, 1.000000000000000000 ) ) ;
#7446 = AXIS2_PLACEMENT_3D ( 'NONE', #4191, #3592, #7382 ) ;
#7447 = VECTOR ( 'NONE', #2660, 39.37007874015748143 ) ;
#7448 = CIRCLE ( 'NONE', #4925, 0.3625000012227142521 ) ;
#7449 = DIRECTION ( 'NONE',  ( -0.000000000000000000, -0.000000000000000000, -1.000000000000000000 ) ) ;
#7450 = DIRECTION ( 'NONE',  ( 1.000000000000000000, 0.000000000000000000, 0.000000000000000000 ) ) ;
#7451 = DIRECTION ( 'NONE',  ( -0.000000000000000000, -1.000000000000000000, -0.000000000000000000 ) ) ;
#7452 = ORIENTED_EDGE ( 'NONE', *, *, #2782, .F. ) ;
#7453 = LINE ( 'NONE', #1187, #5945 ) ;
#7454 =( NAMED_UNIT ( * ) SI_UNIT ( $, .STERADIAN. ) SOLID_ANGLE_UNIT ( ) );
#7455 = CARTESIAN_POINT ( 'NONE',  ( 0.000000000000000000, 5.113999999999999879, -2.750000000000000444 ) ) ;
#7456 = AXIS2_PLACEMENT_3D ( 'NONE', #91, #131, #2648 ) ;
#7457 = DATE_AND_TIME ( #1812, #7221 ) ;
#7458 = ORIENTED_EDGE ( 'NONE', *, *, #2724, .T. ) ;
#7459 = DIRECTION ( 'NONE',  ( -0.7071067811865554553, -1.586444216266441231E-14, -0.7071067811865394681 ) ) ;
#7460 = CC_DESIGN_DATE_AND_TIME_ASSIGNMENT ( #1836, #1991, ( #1242 ) ) ;
#7461 = ORIENTED_EDGE ( 'NONE', *, *, #887, .F. ) ;
#7462 = AXIS2_PLACEMENT_3D ( 'NONE', #1969, #1887, #23 ) ;
#7463 = PLANE ( 'NONE',  #3459 ) ;
#7464 = DIRECTION ( 'NONE',  ( 0.000000000000000000, 0.000000000000000000, -1.000000000000000000 ) ) ;
#7465 = FACE_OUTER_BOUND ( 'NONE', #517, .T. ) ;
#7466 = ORIENTED_EDGE ( 'NONE', *, *, #6405, .T. ) ;
#7467 =( BOUNDED_CURVE ( )  B_SPLINE_CURVE ( 2, ( #3606, #2337, #491, #5987, #4831, #5477, #3648 ),
 .UNSPECIFIED., .F., .F. ) 
 B_SPLINE_CURVE_WITH_KNOTS ( ( 3, 2, 2, 3 ),
 ( 9.875789629141308064E-12, 0.01898937877657074641, 0.04622957261936486151, 0.05624330786770232599 ),
 .UNSPECIFIED. ) 
 CURVE ( )  GEOMETRIC_REPRESENTATION_ITEM ( )  RATIONAL_B_SPLINE_CURVE ( ( 0.8763122937754233011, 0.7958215605093268419, 1.000000000000000000, 0.7071067811865479058, 1.000000000000000000, 0.8923298723145043354, 0.8638207196954514888 ) ) 
 REPRESENTATION_ITEM ( '' )  );
#7468 = EDGE_LOOP ( 'NONE', ( #5664, #2248, #5756, #5391 ) ) ;
#7469 = CC_DESIGN_PERSON_AND_ORGANIZATION_ASSIGNMENT ( #2463, #6213, ( #4922 ) ) ;
#7470 = DIRECTION ( 'NONE',  ( 0.000000000000000000, 0.000000000000000000, 1.000000000000000000 ) ) ;
#7471 = PLANE ( 'NONE',  #4875 ) ;
#7472 = EDGE_CURVE ( 'NONE', #3397, #4502, #7419, .T. ) ;
#7473 = CARTESIAN_POINT ( 'NONE',  ( 1.500000000000000444, 5.414000000000000590, -2.750000000000000444 ) ) ;
#7474 = CARTESIAN_POINT ( 'NONE',  ( 1.187500000000000000, 4.988125073052579239, 4.328661356714555097 ) ) ;
#7475 = ADVANCED_FACE ( 'NONE', ( #3501 ), #6226, .T. ) ;
#7476 = ORIENTED_EDGE ( 'NONE', *, *, #2684, .T. ) ;
#7478 = APPLICATION_PROTOCOL_DEFINITION ( 'international standard', 'config_control_design', 1994, #1532 ) ;
#7477 = CC_DESIGN_SECURITY_CLASSIFICATION ( #1319, ( #6576 ) ) ;
#7479 = LINE ( 'NONE', #514, #7288 ) ;
#7480 = EDGE_CURVE ( 'NONE', #2826, #3433, #6880, .T. ) ;
#7481 = DIRECTION ( 'NONE',  ( 0.000000000000000000, 0.000000000000000000, 1.000000000000000000 ) ) ;
#7482 = CARTESIAN_POINT ( 'NONE',  ( 1.187499999999999778, 5.002317768095269734, 4.083473622031662309 ) ) ;
#7483 = LINE ( 'NONE', #604, #6375 ) ;
#7484 = ORIENTED_EDGE ( 'NONE', *, *, #791, .T. ) ;
#7485 = DATE_AND_TIME ( #6870, #7939 ) ;
#7486 = DIRECTION ( 'NONE',  ( 0.7071067811865474617, -0.000000000000000000, 0.7071067811865474617 ) ) ;
#7487 = CALENDAR_DATE ( 2026, 8, 10 ) ;
#7488 = EDGE_CURVE ( 'NONE', #1366, #1186, #7626, .T. ) ;
#7489 = ADVANCED_FACE ( 'NONE', ( #6801 ), #3685, .T. ) ;
#7490 = DIRECTION ( 'NONE',  ( -0.000000000000000000, 0.000000000000000000, 1.000000000000000000 ) ) ;
#7491 = FACE_OUTER_BOUND ( 'NONE', #2856, .T. ) ;
#7492 = CARTESIAN_POINT ( 'NONE',  ( 0.000000000000000000, 5.160877715062512472, 6.858307716807694909 ) ) ;
#7493 = ORIENTED_EDGE ( 'NONE', *, *, #3599, .T. ) ;
#7494 = CARTESIAN_POINT ( 'NONE',  ( -0.6866307324975362558, 4.251743418646740658, 8.149316802294766404 ) ) ;
#7495 = LINE ( 'NONE', #4993, #2808 ) ;
#7496 = CARTESIAN_POINT ( 'NONE',  ( -3.987046614173228587, 3.753500037802127043, 8.231249998505111520 ) ) ;
#7497 = APPROVAL_ROLE ( '' ) ;
#7498 = ORIENTED_EDGE ( 'NONE', *, *, #7472, .F. ) ;
#7499 = CARTESIAN_POINT ( 'NONE',  ( 3.484120143574221651E-16, 0.000000000000000000, 2.845000000000001528 ) ) ;
#7500 = PRODUCT_DEFINITION_SHAPE ( 'NONE', 'NONE',  #1419 ) ;
#7501 = ORIENTED_EDGE ( 'NONE', *, *, #7872, .T. ) ;
#7502 = LOCAL_TIME ( 0, 37, 23.00000000000000000, #3426 ) ;
#7503 = CARTESIAN_POINT ( 'NONE',  ( -2.750000000000000444, 8.719000000000002970, 3.823750000000002647 ) ) ;
#7504 = DIRECTION ( 'NONE',  ( -1.000000000000000000, 0.000000000000000000, -2.606890220986081510E-17 ) ) ;
#7505 = CARTESIAN_POINT ( 'NONE',  ( -1.187499999435510212, 4.987711023622046547, 4.083473622047245399 ) ) ;
#7506 = ORIENTED_EDGE ( 'NONE', *, *, #7524, .F. ) ;
#7507 = EDGE_LOOP ( 'NONE', ( #4230, #1126, #1815, #1204 ) ) ;
#7508 = LINE ( 'NONE', #6901, #974 ) ;
#7509 = CC_DESIGN_PERSON_AND_ORGANIZATION_ASSIGNMENT ( #6884, #1401, ( #2206 ) ) ;
#7510 = CARTESIAN_POINT ( 'NONE',  ( -0.8694070078740159246, 2.427999212598427103, -5.651320433070869953 ) ) ;
#7511 = CARTESIAN_POINT ( 'NONE',  ( 0.000000000000000000, 5.414000000000000590, 0.1250000000000000278 ) ) ;
#7512 = ORIENTED_EDGE ( 'NONE', *, *, #1955, .T. ) ;
#7513 = PERSON_AND_ORGANIZATION_ROLE ( 'classification_officer' ) ;
#7514 = DIRECTION ( 'NONE',  ( 0.000000000000000000, 0.000000000000000000, 1.000000000000000000 ) ) ;
#7515 = ORIENTED_EDGE ( 'NONE', *, *, #3280, .F. ) ;
#7516 = CARTESIAN_POINT ( 'NONE',  ( -4.462046614173229564, 3.753500037802127043, 8.231249998505111520 ) ) ;
#7517 = CARTESIAN_POINT ( 'NONE',  ( 1.187500000000000222, 7.339000000000003077, 5.236250000000000959 ) ) ;
#7518 = CARTESIAN_POINT ( 'NONE',  ( 0.000000000000000000, 3.950000000000001954, 3.956250000000000266 ) ) ;
#7519 = VERTEX_POINT ( 'NONE', #8130 ) ;
#7520 = PERSON_AND_ORGANIZATION ( #7862, #8117 ) ;
#7521 = LINE ( 'NONE', #1214, #1639 ) ;
#7522 = CONTEXT_DEPENDENT_SHAPE_REPRESENTATION ( #5598, #5882 ) ;
#7523 = CARTESIAN_POINT ( 'NONE',  ( 2.349999998660270872, 3.550000000000001155, -1.169467086614173645 ) ) ;
#7524 = EDGE_CURVE ( 'NONE', #1240, #7663, #4297, .T. ) ;
#7525 = ADVANCED_FACE ( 'NONE', ( #3190 ), #3066, .F. ) ;
#7526 = CARTESIAN_POINT ( 'NONE',  ( -3.987046614173229475, 3.765347506452386916, 8.164015047692851468 ) ) ;
#7527 = EDGE_CURVE ( 'NONE', #1578, #4491, #5394, .T. ) ;
#7528 = PLANE ( 'NONE',  #2270 ) ;
#7529 = ORIENTED_EDGE ( 'NONE', *, *, #1931, .F. ) ;
#7530 = CARTESIAN_POINT ( 'NONE',  ( -8.751021560936518753E-10, 1.000000000000000222, 5.750408897959578548E-10 ) ) ;
#7531 = DIRECTION ( 'NONE',  ( 1.000000000000000000, 0.000000000000000000, 0.000000000000000000 ) ) ;
#7532 = DIRECTION ( 'NONE',  ( 0.000000000000000000, 0.000000000000000000, 1.000000000000000000 ) ) ;
#7533 = DATE_AND_TIME ( #7616, #6909 ) ;
#7534 = EDGE_LOOP ( 'NONE', ( #3816, #6418, #793, #6351, #7476, #3953, #1978 ) ) ;
#7535 = CARTESIAN_POINT ( 'NONE',  ( 2.750000000000000444, 8.729000000000002757, 4.313750000000002416 ) ) ;
#7536 = EDGE_CURVE ( 'NONE', #8045, #3948, #3573, .T. ) ;
#7537 = VECTOR ( 'NONE', #4666, 39.37007874015748854 ) ;
#7538 = LOCAL_TIME ( 0, 37, 23.00000000000000000, #3679 ) ;
#7539 = CYLINDRICAL_SURFACE ( 'NONE', #6620, 0.2625000000000008438 ) ;
#7540 = VECTOR ( 'NONE', #6857, 39.37007874015748854 ) ;
#7541 = AXIS2_PLACEMENT_3D ( 'NONE', #592, #3630, #4394 ) ;
#7542 = FACE_OUTER_BOUND ( 'NONE', #6060, .T. ) ;
#7543 = CC_DESIGN_APPROVAL ( #3007, ( #1877 ) ) ;
#7544 = ORIENTED_EDGE ( 'NONE', *, *, #2725, .F. ) ;
#7545 = VERTEX_POINT ( 'NONE', #4989 ) ;
#7546 = EDGE_CURVE ( 'NONE', #2207, #1601, #6700, .T. ) ;
#7547 = AXIS2_PLACEMENT_3D ( 'NONE', #3269, #142, #2659 ) ;
#7548 = CARTESIAN_POINT ( 'NONE',  ( 3.987953385826772390, 4.134652525424356462, 8.164015047692018356 ) ) ;
#7549 = CARTESIAN_POINT ( 'NONE',  ( 1.277972679321882632, 3.650152906200382130, -5.108750000000001457 ) ) ;
#7550 = VECTOR ( 'NONE', #6655, 39.37007874015748143 ) ;
#7551 = CARTESIAN_POINT ( 'NONE',  ( 1.187500000000000000, 4.823830681599543979, 5.419287633353158107 ) ) ;
#7552 = ORIENTED_EDGE ( 'NONE', *, *, #7239, .T. ) ;
#7553 = PERSON_AND_ORGANIZATION ( #7862, #8117 ) ;
#7554 = VECTOR ( 'NONE', #3152, 39.37007874015748143 ) ;
#7555 = DIRECTION ( 'NONE',  ( 0.000000000000000000, 0.000000000000000000, 1.000000000000000000 ) ) ;
#7556 = ORIENTED_EDGE ( 'NONE', *, *, #7317, .F. ) ;
#7557 = CC_DESIGN_PERSON_AND_ORGANIZATION_ASSIGNMENT ( #3902, #801, ( #3008 ) ) ;
#7558 = VECTOR ( 'NONE', #7486, 39.37007874015748854 ) ;
#7559 = VECTOR ( 'NONE', #4027, 39.37007874015748143 ) ;
#7560 = AXIS2_PLACEMENT_3D ( 'NONE', #1276, #4954, #1310 ) ;
#7561 = CARTESIAN_POINT ( 'NONE',  ( -2.749999999999999556, 7.964000000000000412, 2.411250000000000338 ) ) ;
#7562 = EDGE_LOOP ( 'NONE', ( #1634, #5246, #287, #3605 ) ) ;
#7563 = PERSON_AND_ORGANIZATION ( #7862, #8117 ) ;
#7564 = FACE_OUTER_BOUND ( 'NONE', #981, .T. ) ;
#7565 = APPROVAL_STATUS ( 'not_yet_approved' ) ;
#7566 = DIRECTION ( 'NONE',  ( 0.000000000000000000, 0.000000000000000000, 1.000000000000000000 ) ) ;
#7567 = AXIS2_PLACEMENT_3D ( 'NONE', #5815, #2777, #3949 ) ;
#7568 = VECTOR ( 'NONE', #7246, 39.37007874015748143 ) ;
#7569 = CARTESIAN_POINT ( 'NONE',  ( -1.198957880909643725, 2.499999999928966599, 2.750000000000000444 ) ) ;
#7570 = CARTESIAN_POINT ( 'NONE',  ( -4.066213280839896527, 3.516000035344541974, 8.231249998505111520 ) ) ;
#7571 = EDGE_LOOP ( 'NONE', ( #2775, #535, #4960, #355 ) ) ;
#7572 = CARTESIAN_POINT ( 'NONE',  ( -1.187500000000000222, 4.160767401574803515, 6.858307716535433585 ) ) ;
#7573 = ADVANCED_FACE ( 'NONE', ( #6308, #4915 ), #652, .T. ) ;
#7574 = LENGTH_MEASURE_WITH_UNIT ( LENGTH_MEASURE( 0.02539999999999999897 ), #5033 );
#7575 = CARTESIAN_POINT ( 'NONE',  ( -1.187499999999999334, 4.622310746201133469, 6.124573350433617946 ) ) ;
#7576 = PERSON_AND_ORGANIZATION ( #7862, #8117 ) ;
#7577 = VERTEX_POINT ( 'NONE', #1222 ) ;
#7578 = CARTESIAN_POINT ( 'NONE',  ( 0.000000000000000000, 2.762500000000000178, 6.956250000000000711 ) ) ;
#7579 = EDGE_CURVE ( 'NONE', #2772, #2861, #1227, .T. ) ;
#7580 =( BOUNDED_CURVE ( )  B_SPLINE_CURVE ( 2, ( #3754, #5060, #2526, #7599, #7561, #1907, #5846, #5214, #7722 ),
 .UNSPECIFIED., .F., .F. ) 
 B_SPLINE_CURVE_WITH_KNOTS ( ( 3, 2, 2, 2, 3 ),
 ( 0.000000000000000000, 0.01376350590101864911, 0.04131120848487213754, 0.06885891106872543688, 0.07294458654364180394 ),
 .UNSPECIFIED. ) 
 CURVE ( )  GEOMETRIC_REPRESENTATION_ITEM ( )  RATIONAL_B_SPLINE_CURVE ( ( 0.8535534732088591037, 0.8536633850130519452, 1.000000000000000000, 0.7071067811865479058, 1.000000000000000000, 0.7071067811865479058, 1.000000000000000000, 0.9565602018087399072, 0.9260057553135151442 ) ) 
 REPRESENTATION_ITEM ( '' )  );
#7581 = DIRECTION ( 'NONE',  ( 0.000000000000000000, -0.000000000000000000, 1.000000000000000000 ) ) ;
#7582 = AXIS2_PLACEMENT_3D ( 'NONE', #2159, #930, #6425 ) ;
#7583 = AXIS2_PLACEMENT_3D ( 'NONE', #6892, #1849, #7620 ) ;
#7584 = DIRECTION ( 'NONE',  ( 0.7071067811865475727, 0.000000000000000000, -0.7071067811865475727 ) ) ;
#7585 = ORIENTED_EDGE ( 'NONE', *, *, #2443, .T. ) ;
#7586 = VERTEX_POINT ( 'NONE', #614 ) ;
#7587 = EDGE_CURVE ( 'NONE', #1938, #5712, #3962, .T. ) ;
#7588 = LINE ( 'NONE', #7886, #2411 ) ;
#7589 = ADVANCED_FACE ( 'NONE', ( #5072 ), #7528, .T. ) ;
#7590 = CARTESIAN_POINT ( 'NONE',  ( 1.113928741201104078, 3.255531826294225883, -5.108750000000003233 ) ) ;
#7591 = VERTEX_POINT ( 'NONE', #6959 ) ;
#7592 = VECTOR ( 'NONE', #1191, 39.37007874015748143 ) ;
#7593 = CALENDAR_DATE ( 2026, 8, 10 ) ;
#7594 = CARTESIAN_POINT ( 'NONE',  ( 3.987953385826772390, 3.766991497692264712, 8.302809606439794265 ) ) ;
#7595 = CARTESIAN_POINT ( 'NONE',  ( 1.198957881890679422, 2.500000000000000000, 2.749999999536767437 ) ) ;
#7596 = ORIENTED_EDGE ( 'NONE', *, *, #942, .T. ) ;
#7597 = SECURITY_CLASSIFICATION ( '', '', #3842 ) ;
#7598 = DIRECTION ( 'NONE',  ( 0.000000000000000000, -1.000000000000000000, 0.000000000000000000 ) ) ;
#7599 = CARTESIAN_POINT ( 'NONE',  ( -2.749999999999998668, 7.339000000000003077, 2.411250000000000782 ) ) ;
#7600 = DIRECTION ( 'NONE',  ( 0.3026345437736693289, 0.000000000000000000, -0.9531066744677130220 ) ) ;
#7601 = ORIENTED_EDGE ( 'NONE', *, *, #784, .F. ) ;
#7602 = APPROVAL_STATUS ( 'not_yet_approved' ) ;
#7603 = LINE ( 'NONE', #1954, #4644 ) ;
#7604 = PERSON_AND_ORGANIZATION ( #5355, #4511 ) ;
#7605 = DIRECTION ( 'NONE',  ( 0.000000000000000000, -1.000000000000000000, 0.000000000000000000 ) ) ;
#7606 = FACE_BOUND ( 'NONE', #3723, .T. ) ;
#7607 = DIRECTION ( 'NONE',  ( 0.7071067811865474617, 0.7071067811865474617, -0.000000000000000000 ) ) ;
#7608 = CARTESIAN_POINT ( 'NONE',  ( 2.537500000000000533, 2.500000000000000444, 0.000000000000000000 ) ) ;
#7609 = ORIENTED_EDGE ( 'NONE', *, *, #1798, .T. ) ;
#7610 = CARTESIAN_POINT ( 'NONE',  ( -3.987046614173229031, 4.146499994074616779, 8.624249954777603477 ) ) ;
#7611 = CARTESIAN_POINT ( 'NONE',  ( -2.750000000000000444, 7.541160346212514298, 3.714531354832316445 ) ) ;
#7612 = ORIENTED_EDGE ( 'NONE', *, *, #6553, .T. ) ;
#7613 =( NAMED_UNIT ( * ) SI_UNIT ( $, .STERADIAN. ) SOLID_ANGLE_UNIT ( ) );
#7614 = APPROVAL ( #2609, 'UNSPECIFIED' ) ;
#7615 = CARTESIAN_POINT ( 'NONE',  ( -2.750000000000000444, 7.339000000000001300, 4.486250000000000959 ) ) ;
#7616 = CALENDAR_DATE ( 2026, 8, 10 ) ;
#7617 = EDGE_LOOP ( 'NONE', ( #7347, #1100, #5057 ) ) ;
#7618 = CARTESIAN_POINT ( 'NONE',  ( -2.740000000000006430, 1.956931634677146971E-15, 3.323750000000001759 ) ) ;
#7619 = DIRECTION ( 'NONE',  ( 0.000000000000000000, 1.000000000000000000, 0.000000000000000000 ) ) ;
#7620 = DIRECTION ( 'NONE',  ( 1.000000000000000000, 0.000000000000000000, 0.000000000000000000 ) ) ;
#7621 = LINE ( 'NONE', #3202, #1505 ) ;
#7622 = DIRECTION ( 'NONE',  ( -1.000000000000000000, -0.000000000000000000, -0.000000000000000000 ) ) ;
#7623 = ORIENTED_EDGE ( 'NONE', *, *, #5301, .T. ) ;
#7624 = ORIENTED_EDGE ( 'NONE', *, *, #317, .F. ) ;
#7625 = DESIGN_CONTEXT ( 'detailed design', #1532, 'design' ) ;
#7626 =( BOUNDED_CURVE ( )  B_SPLINE_CURVE ( 3, ( #7492, #565, #3765, #4454 ),
 .UNSPECIFIED., .F., .F. ) 
 B_SPLINE_CURVE_WITH_KNOTS ( ( 4, 4 ),
 ( 0.9667407784957844363, 1.000000000000000000 ),
 .UNSPECIFIED. ) 
 CURVE ( )  GEOMETRIC_REPRESENTATION_ITEM ( )  RATIONAL_B_SPLINE_CURVE ( ( 0.9996521287670052658, 0.9997640965207306163, 0.9998800535983954907, 1.000000000000000000 ) ) 
 REPRESENTATION_ITEM ( '' )  );
#7627 = APPROVAL_PERSON_ORGANIZATION ( #1681, #6214, #1802 ) ;
#7628 = CARTESIAN_POINT ( 'NONE',  ( 3.987953385826771946, 4.027703970067857853, 8.050752829671607103 ) ) ;
#7629 = CARTESIAN_POINT ( 'NONE',  ( 1.116010524871317244, 4.642101986333586616, -5.108750000000002345 ) ) ;
#7630 = LINE ( 'NONE', #4516, #1255 ) ;
#7631 = CARTESIAN_POINT ( 'NONE',  ( 3.987953385826772390, 3.836846444618124075, 8.391936332831416934 ) ) ;
#7632 = ORIENTED_EDGE ( 'NONE', *, *, #3431, .T. ) ;
#7633 = LOCAL_TIME ( 0, 37, 23.00000000000000000, #6112 ) ;
#7634 = EDGE_CURVE ( 'NONE', #6439, #7338, #7806, .T. ) ;
#7635 = LOCAL_TIME ( 0, 37, 23.00000000000000000, #1913 ) ;
#7636 = DIRECTION ( 'NONE',  ( -0.000000000000000000, 1.000000000000000000, -0.000000000000000000 ) ) ;
#7637 = EDGE_LOOP ( 'NONE', ( #3638, #7826 ) ) ;
#7638 = APPROVAL_ROLE ( '' ) ;
#7639 = PLANE ( 'NONE',  #2166 ) ;
#7640 = DATE_AND_TIME ( #3146, #6217 ) ;
#7641 = CARTESIAN_POINT ( 'NONE',  ( 4.462953385826773811, 3.674333370316266389, 8.231249998505111520 ) ) ;
#7642 = DIRECTION ( 'NONE',  ( -0.000000000000000000, 1.000000000000000000, 0.000000000000000000 ) ) ;
#7643 = EDGE_CURVE ( 'NONE', #3600, #3210, #4222, .T. ) ;
#7644 = ORIENTED_EDGE ( 'NONE', *, *, #830, .T. ) ;
#7645 = CC_DESIGN_SECURITY_CLASSIFICATION ( #1197, ( #8194 ) ) ;
#7646 = DIRECTION ( 'NONE',  ( -1.000000000000000000, 0.000000000000000000, 0.000000000000000000 ) ) ;
#7647 = DIRECTION ( 'NONE',  ( -0.000000000000000000, 1.000000000000000000, -0.000000000000000000 ) ) ;
#7648 = CARTESIAN_POINT ( 'NONE',  ( -3.987046614173230363, 4.068613208432641848, 8.387951386028037248 ) ) ;
#7649 = EDGE_LOOP ( 'NONE', ( #1460, #7601, #6158, #1818, #174, #809, #5518, #7119, #6116, #1223, #2442, #6705, #4236, #3028, #3982, #5772, #5178 ) ) ;
#7650 = DIRECTION ( 'NONE',  ( 1.000000000000000000, 0.000000000000000000, -0.000000000000000000 ) ) ;
#7651 = DIRECTION ( 'NONE',  ( 0.7071067811865442421, 8.659560562354893415E-17, -0.7071067811865507924 ) ) ;
#7652 = LINE ( 'NONE', #4619, #3622 ) ;
#7653 = DATE_AND_TIME ( #620, #2338 ) ;
#7654 = EDGE_LOOP ( 'NONE', ( #3531, #6409, #5668, #6574, #2495, #4434, #1155 ) ) ;
#7655 = CC_DESIGN_PERSON_AND_ORGANIZATION_ASSIGNMENT ( #3100, #8067, ( #5941 ) ) ;
#7656 = PLANE ( 'NONE',  #5015 ) ;
#7657 =( LENGTH_UNIT ( ) NAMED_UNIT ( * ) SI_UNIT ( $, .METRE. ) );
#7658 = DIRECTION ( 'NONE',  ( 0.000000000000000000, 0.7071067811865282549, 0.7071067811865667796 ) ) ;
#7659 = ORIENTED_EDGE ( 'NONE', *, *, #7314, .F. ) ;
#7660 = CARTESIAN_POINT ( 'NONE',  ( -0.6955978521287337069, 3.669434091866875303, 8.092097759609567120 ) ) ;
#7661 = APPROVAL_PERSON_ORGANIZATION ( #6258, #8089, #4943 ) ;
#7662 = FACE_OUTER_BOUND ( 'NONE', #3789, .T. ) ;
#7663 = VERTEX_POINT ( 'NONE', #5109 ) ;
#7664 = AXIS2_PLACEMENT_3D ( 'NONE', #969, #1738, #3038 ) ;
#7665 = APPROVAL_PERSON_ORGANIZATION ( #2562, #4714, #1790 ) ;
#7666 = CARTESIAN_POINT ( 'NONE',  ( 0.000000000000000000, 0.000000000000000000, -2.845000000000001528 ) ) ;
#7667 = CARTESIAN_POINT ( 'NONE',  ( 0.7665824091426678422, 5.016224573579987300, -5.108750000000005009 ) ) ;
#7668 = EDGE_CURVE ( 'NONE', #231, #1601, #1127, .T. ) ;
#7669 = CARTESIAN_POINT ( 'NONE',  ( 3.987953385826773278, 3.783676849830679867, 8.335940882964230525 ) ) ;
#7670 = EDGE_CURVE ( 'NONE', #5362, #941, #2968, .T. ) ;
#7671 = AXIS2_PLACEMENT_3D ( 'NONE', #5375, #2921, #4105 ) ;
#7672 = VERTEX_POINT ( 'NONE', #3701 ) ;
#7673 = VECTOR ( 'NONE', #5460, 39.37007874015748143 ) ;
#7674 = SECURITY_CLASSIFICATION ( '', '', #2134 ) ;
#7675 = EDGE_CURVE ( 'NONE', #4344, #5123, #8022, .T. ) ;
#7676 = VECTOR ( 'NONE', #4961, 39.37007874015748143 ) ;
#7677 = AXIS2_PLACEMENT_3D ( 'NONE', #6194, #1817, #4309 ) ;
#7678 = DIRECTION ( 'NONE',  ( 0.000000000000000000, 0.000000000000000000, 1.000000000000000000 ) ) ;
#7679 = LINE ( 'NONE', #1950, #1113 ) ;
#7680 = ORIENTED_EDGE ( 'NONE', *, *, #8012, .T. ) ;
#7681 = EDGE_CURVE ( 'NONE', #4377, #843, #5499, .T. ) ;
#7682 = DATE_TIME_ROLE ( 'classification_date' ) ;
#7683 = FACE_OUTER_BOUND ( 'NONE', #1039, .T. ) ;
#7684 = DATE_TIME_ROLE ( 'classification_date' ) ;
#7685 = CARTESIAN_POINT ( 'NONE',  ( 0.7078558382242211566, 3.701833123853966789, 8.040237954860639746 ) ) ;
#7686 = CARTESIAN_POINT ( 'NONE',  ( 0.7417920657368231030, 4.061067302434975268, 8.523525407967506240 ) ) ;
#7687 = DIRECTION ( 'NONE',  ( 0.000000000000000000, -1.000000000000000000, 0.000000000000000000 ) ) ;
#7688 = AXIS2_PLACEMENT_3D ( 'NONE', #4012, #5321, #1566 ) ;
#7689 = CIRCLE ( 'NONE', #7264, 2.619834133858267577 ) ;
#7690 = ORIENTED_EDGE ( 'NONE', *, *, #5505, .T. ) ;
#7691 = CARTESIAN_POINT ( 'NONE',  ( -3.987046614173227699, 3.763524128032367688, 8.169134493242211192 ) ) ;
#7692 = CARTESIAN_POINT ( 'NONE',  ( -0.8527717963921712663, 5.380045629635501925, 4.083473622047245399 ) ) ;
#7693 = VECTOR ( 'NONE', #7349, 39.37007874015748854 ) ;
#7694 = CARTESIAN_POINT ( 'NONE',  ( -3.987046614173229475, 3.768538842735829952, 8.306660907471561828 ) ) ;
#7695 = ORIENTED_EDGE ( 'NONE', *, *, #6238, .T. ) ;
#7696 = CARTESIAN_POINT ( 'NONE',  ( -1.500000000000000444, 5.639000000000001123, -2.750000000000000444 ) ) ;
#7697 = ORIENTED_EDGE ( 'NONE', *, *, #1005, .F. ) ;
#7698 = DIRECTION ( 'NONE',  ( 0.0005594472316432180879, -8.183956524382551076E-17, 0.9999998435093852001 ) ) ;
#7699 = ORGANIZATION ( 'NAUO-ORG5', 'UNSPECIFIED', 'UNSPECIFIED' ) ;
#7700 = CARTESIAN_POINT ( 'NONE',  ( -1.187500000000000222, 4.294835038531924276, 6.747773014656689661 ) ) ;
#7701 = APPROVAL_STATUS ( 'not_yet_approved' ) ;
#7702 = ORIENTED_EDGE ( 'NONE', *, *, #4799, .F. ) ;
#7703 = CIRCLE ( 'NONE', #2690, 0.3625000000000019318 ) ;
#7704 = AXIS2_PLACEMENT_3D ( 'NONE', #356, #2531, #8035 ) ;
#7705 = CARTESIAN_POINT ( 'NONE',  ( 2.740000000000001545, 7.964000000000000412, 3.823750000000002647 ) ) ;
#7706 = DIRECTION ( 'NONE',  ( -0.5773502691896257311, 0.5773502691896257311, -0.5773502691896257311 ) ) ;
#7707 = AXIS2_PLACEMENT_3D ( 'NONE', #5128, #3334, #5956 ) ;
#7708 = EDGE_LOOP ( 'NONE', ( #6434, #1624, #6280, #7732 ) ) ;
#7709 = APPROVAL ( #5984, 'UNSPECIFIED' ) ;
#7710 = CARTESIAN_POINT ( 'NONE',  ( 0.7457411423250316362, 3.867608449240890867, 8.533409342498828210 ) ) ;
#7711 = ORIENTED_EDGE ( 'NONE', *, *, #6059, .T. ) ;
#7712 = DIRECTION ( 'NONE',  ( 0.000000000000000000, 0.000000000000000000, 1.000000000000000000 ) ) ;
#7713 = CARTESIAN_POINT ( 'NONE',  ( 0.9907400445861593852, 4.815212283617434252, -5.108749999999999680 ) ) ;
#7714 = DIRECTION ( 'NONE',  ( -0.5773502691896258421, 0.5773502691896258421, -0.5773502691896258421 ) ) ;
#7715 = CC_DESIGN_DATE_AND_TIME_ASSIGNMENT ( #2237, #7934, ( #1030 ) ) ;
#7716 = CARTESIAN_POINT ( 'NONE',  ( 3.987953385826773278, 4.079363137581865750, 8.379777743322501138 ) ) ;
#7717 = CIRCLE ( 'NONE', #4664, 0.4312500000000004663 ) ;
#7718 = ORIENTED_EDGE ( 'NONE', *, *, #601, .F. ) ;
#7719 = DIRECTION ( 'NONE',  ( -0.000000000000000000, 1.000000000000000000, -0.000000000000000000 ) ) ;
#7720 = EDGE_CURVE ( 'NONE', #789, #2992, #6703, .T. ) ;
#7721 = CARTESIAN_POINT ( 'NONE',  ( 2.537500000000000533, 2.500000000000000444, 0.000000000000000000 ) ) ;
#7722 = CARTESIAN_POINT ( 'NONE',  ( -2.750000000000000444, 8.574153543306394454, 3.323750000003751648 ) ) ;
#7723 = VERTEX_POINT ( 'NONE', #6127 ) ;
#7724 = APPROVAL_DATE_TIME ( #7807, #7614 ) ;
#7725 = EDGE_CURVE ( 'NONE', #2362, #3476, #1369, .T. ) ;
#7726 = LINE ( 'NONE', #3469, #7149 ) ;
#7727 = SECURITY_CLASSIFICATION_LEVEL ( 'unclassified' ) ;
#7728 = CARTESIAN_POINT ( 'NONE',  ( 2.349999998660270872, 3.550000000000001155, 2.790532913385826763 ) ) ;
#7729 = CARTESIAN_POINT ( 'NONE',  ( 0.7456179150311872394, 4.031565731729908286, 8.533094314006415715 ) ) ;
#7730 =( BOUNDED_CURVE ( )  B_SPLINE_CURVE ( 3, ( #6038, #2799, #6627, #7328 ),
 .UNSPECIFIED., .F., .F. ) 
 B_SPLINE_CURVE_WITH_KNOTS ( ( 4, 4 ),
 ( 4.504740859246951633E-12, 0.04207438291838416777 ),
 .UNSPECIFIED. ) 
 CURVE ( )  GEOMETRIC_REPRESENTATION_ITEM ( )  RATIONAL_B_SPLINE_CURVE ( ( 0.5046980198592107003, 0.5343480760378280792, 0.6993327790067819238, 0.9996521287660721233 ) ) 
 REPRESENTATION_ITEM ( '' )  );
#7731 = APPROVAL_PERSON_ORGANIZATION ( #1967, #5459, #1280 ) ;
#7732 = ORIENTED_EDGE ( 'NONE', *, *, #670, .T. ) ;
#7733 = CARTESIAN_POINT ( 'NONE',  ( -3.987046614173228587, 4.136475903844373470, 8.293365503768981739 ) ) ;
#7734 = ORIENTED_EDGE ( 'NONE', *, *, #7755, .T. ) ;
#7735 = CARTESIAN_POINT ( 'NONE',  ( 0.000000000000000000, 2.661265787401576155, 3.956250000000001155 ) ) ;
#7736 = ORIENTED_EDGE ( 'NONE', *, *, #4387, .T. ) ;
#7737 =( CONVERSION_BASED_UNIT ( 'INCH', #778 ) LENGTH_UNIT ( ) NAMED_UNIT ( #8169 ) );
#7738 = ADVANCED_FACE ( 'NONE', ( #6781 ), #7471, .T. ) ;
#7739 = LINE ( 'NONE', #2092, #6082 ) ;
#7740 = LINE ( 'NONE', #8084, #5707 ) ;
#7741 = APPROVAL_DATE_TIME ( #5865, #1365 ) ;
#7742 = ORIENTED_EDGE ( 'NONE', *, *, #4131, .F. ) ;
#7743 = ADVANCED_FACE ( 'NONE', ( #6744 ), #8108, .T. ) ;
#7744 = CARTESIAN_POINT ( 'NONE',  ( -6.890193713091687007E-11, 5.025000000000000355, 3.440250000000001140 ) ) ;
#7745 = LINE ( 'NONE', #2097, #6206 ) ;
#7746 = CARTESIAN_POINT ( 'NONE',  ( 2.750000000000000444, 7.964000000000000412, 2.411250000000000338 ) ) ;
#7747 = LINE ( 'NONE', #2715, #6999 ) ;
#7748 = ORIENTED_EDGE ( 'NONE', *, *, #388, .F. ) ;
#7749 = DATE_TIME_ROLE ( 'creation_date' ) ;
#7750 = VERTEX_POINT ( 'NONE', #6163 ) ;
#7751 = PLANE ( 'NONE',  #4213 ) ;
#7752 = CARTESIAN_POINT ( 'NONE',  ( 3.987953385826772390, 3.799477730091489036, 8.104614619826481459 ) ) ;
#7753 = CARTESIAN_POINT ( 'NONE',  ( -2.750000000000000888, 7.974000000000001087, 3.813750000000002416 ) ) ;
#7754 = DIRECTION ( 'NONE',  ( 3.865154999631033652E-14, -0.7071067811865474617, -0.7071067811865474617 ) ) ;
#7755 = EDGE_CURVE ( 'NONE', #7113, #212, #2820, .T. ) ;
#7756 = CARTESIAN_POINT ( 'NONE',  ( 1.500000000000000444, 5.414000000000000590, 0.1249999999999999861 ) ) ;
#7757 = VERTEX_POINT ( 'NONE', #2359 ) ;
#7758 = APPROVAL ( #6068, 'UNSPECIFIED' ) ;
#7759 = CC_DESIGN_APPROVAL ( #6072, ( #1058 ) ) ;
#7760 = CYLINDRICAL_SURFACE ( 'NONE', #4234, 3.874999999025058539 ) ;
#7761 = ORIENTED_EDGE ( 'NONE', *, *, #7239, .F. ) ;
#7762 = DATE_AND_TIME ( #763, #1996 ) ;
#7763 = DIRECTION ( 'NONE',  ( 0.9917930140139561423, -0.000000000000000000, -0.1278538906451907597 ) ) ;
#7764 = DATE_AND_TIME ( #7081, #8047 ) ;
#7765 = CARTESIAN_POINT ( 'NONE',  ( 4.067120052493439886, 3.516000035344543306, 8.231249998505111520 ) ) ;
#7766 = CARTESIAN_POINT ( 'NONE',  ( 2.724999998660272205, 3.550000000000001155, -1.169467086614173645 ) ) ;
#7767 = ADVANCED_FACE ( 'N', ( #4812 ), #3407, .T. ) ;
#7768 = ORIENTED_EDGE ( 'NONE', *, *, #1704, .T. ) ;
#7769 = DIRECTION ( 'NONE',  ( -0.000000000000000000, -0.000000000000000000, 1.000000000000000000 ) ) ;
#7770 = CARTESIAN_POINT ( 'NONE',  ( -3.987046614173227699, 4.118031710298097892, 8.333174882269599237 ) ) ;
#7771 = ORIENTED_EDGE ( 'NONE', *, *, #249, .T. ) ;
#7772 = DIRECTION ( 'NONE',  ( -1.000000000000000000, 0.000000000000000000, 0.000000000000000000 ) ) ;
#7773 = DIRECTION ( 'NONE',  ( 0.9615291325111615661, 0.000000000000000000, 0.2747029802028605472 ) ) ;
#7774 =( BOUNDED_SURFACE ( )  B_SPLINE_SURFACE ( 3, 3, ( 
 ( #2388, #4713, #6693, #7365 ),
 ( #459, #5403, #4209, #1692 ),
 ( #7963, #2303, #3617, #4749 ),
 ( #999, #8051, #2955, #6115 ) ),
 .UNSPECIFIED., .F., .F., .T. ) 
 B_SPLINE_SURFACE_WITH_KNOTS ( ( 4, 4 ),
 ( 4, 4 ),
 ( 0.000000000000000000, 1.000000000000000000 ),
 ( 0.000000000000000000, 1.000000000000000000 ),
 .UNSPECIFIED. ) 
 GEOMETRIC_REPRESENTATION_ITEM ( )  RATIONAL_B_SPLINE_SURFACE ( (
 ( 1.000000000000000000, 0.3333333333333334259, 0.3333333333333334259, 1.000000000000000000),
 ( 1.000000000000000000, 0.3333333333333334259, 0.3333333333333334259, 1.000000000000000000),
 ( 1.000000000000000000, 0.3333333333333334259, 0.3333333333333334259, 1.000000000000000000),
 ( 1.000000000000000000, 0.3333333333333334259, 0.3333333333333334259, 1.000000000000000000) ) ) 
 REPRESENTATION_ITEM ( '' )  SURFACE ( )  );
#7775 = CARTESIAN_POINT ( 'NONE',  ( 0.7499999999999993339, 3.950000000000000178, 7.231250000000000178 ) ) ;
#7776 = EDGE_CURVE ( 'NONE', #963, #2985, #509, .T. ) ;
#7777 = CARTESIAN_POINT ( 'NONE',  ( 0.7499999999999993339, 3.950000000000000178, 8.543750000000002842 ) ) ;
#7778 = DATE_TIME_ROLE ( 'creation_date' ) ;
#7779 = ORIENTED_EDGE ( 'NONE', *, *, #62, .F. ) ;
#7780 = EDGE_CURVE ( 'NONE', #5858, #3252, #4186, .T. ) ;
#7781 = EDGE_CURVE ( 'NONE', #520, #4455, #6087, .T. ) ;
#7782 = CARTESIAN_POINT ( 'NONE',  ( -0.5437243662217851048, 2.754645391114584729, -5.108750000000005009 ) ) ;
#7783 = CARTESIAN_POINT ( 'NONE',  ( 0.7335700384228724946, 2.500000000438529657, -5.108750000000001457 ) ) ;
#7784 =( LENGTH_UNIT ( ) NAMED_UNIT ( * ) SI_UNIT ( $, .METRE. ) );
#7785 = FACE_OUTER_BOUND ( 'NONE', #3740, .T. ) ;
#7786 = ORIENTED_EDGE ( 'NONE', *, *, #279, .T. ) ;
#7787 = PERSON_AND_ORGANIZATION ( #7862, #8117 ) ;
#7788 = EDGE_CURVE ( 'NONE', #95, #6942, #3560, .T. ) ;
#7789 = VERTEX_POINT ( 'NONE', #2682 ) ;
#7790 = DIRECTION ( 'NONE',  ( -0.000000000000000000, 1.000000000000000000, -0.000000000000000000 ) ) ;
#7791 = CARTESIAN_POINT ( 'NONE',  ( 0.6994518761186668820, 3.679055344357499813, 8.388267944106205576 ) ) ;
#7792 = DESIGN_CONTEXT ( 'detailed design', #1684, 'design' ) ;
#7793 = APPLICATION_CONTEXT ( 'configuration controlled 3d designs of mechanical parts and assemblies' ) ;
#7794 = CARTESIAN_POINT ( 'NONE',  ( 2.537499998660271761, 3.550000000000001155, -1.169467086614173645 ) ) ;
#7795 = DIRECTION ( 'NONE',  ( 1.000000000000000000, -0.000000000000000000, -0.000000000000000000 ) ) ;
#7796 = CARTESIAN_POINT ( 'NONE',  ( 2.537499998660271761, 3.550000000000001155, -1.169467086614173645 ) ) ;
#7797 = ADVANCED_FACE ( 'NONE', ( #5170 ), #1540, .T. ) ;
#7798 = CARTESIAN_POINT ( 'NONE',  ( 2.750000000000000888, 8.729000000000002757, 3.813750000000002416 ) ) ;
#7799 = ORIENTED_EDGE ( 'NONE', *, *, #2493, .T. ) ;
#7800 = MANIFOLD_SOLID_BREP ( 'Imported1', #1897 ) ;
#7801 = AXIS2_PLACEMENT_3D ( 'NONE', #6552, #130, #1050 ) ;
#7802 = SECURITY_CLASSIFICATION ( '', '', #6950 ) ;
#7803 = CARTESIAN_POINT ( 'NONE',  ( 1.198957881665148717, 2.500000000196656025, -2.749999999536767437 ) ) ;
#7804 = CARTESIAN_POINT ( 'NONE',  ( 0.2593509847069561114, 2.344531234934315478, -3.060965062716212159 ) ) ;
#7805 = DIRECTION ( 'NONE',  ( -1.000000000000000000, 0.000000000000000000, 0.000000000000000000 ) ) ;
#7806 = CIRCLE ( 'NONE', #1874, 0.2625000000000008438 ) ;
#7807 = DATE_AND_TIME ( #2729, #5131 ) ;
#7808 = VECTOR ( 'NONE', #1244, 39.37007874015748854 ) ;
#7809 = DIRECTION ( 'NONE',  ( 0.000000000000000000, 0.000000000000000000, -1.000000000000000000 ) ) ;
#7810 = APPROVAL_STATUS ( 'not_yet_approved' ) ;
#7811 = LINE ( 'NONE', #7728, #302 ) ;
#7812 = APPROVAL ( #3759, 'UNKNOWN' ) ;
#7813 = CARTESIAN_POINT ( 'NONE',  ( -1.489119986650662364, 2.223645902236881966, -2.750000000000000444 ) ) ;
#7814 = CARTESIAN_POINT ( 'NONE',  ( -2.750000000000000444, 7.973999999999999311, 3.833750000000001545 ) ) ;
#7815 = AXIS2_PLACEMENT_3D ( 'NONE', #3543, #2885, #4279 ) ;
#7816 = VECTOR ( 'NONE', #907, 39.37007874015748143 ) ;
#7817 = VERTEX_POINT ( 'NONE', #6455 ) ;
#7818 = CARTESIAN_POINT ( 'NONE',  ( -3.987046614173228587, 4.051974939360865058, 8.399350079849284612 ) ) ;
#7819 = EDGE_LOOP ( 'NONE', ( #4132, #3035 ) ) ;
#7820 = FACE_OUTER_BOUND ( 'NONE', #4145, .T. ) ;
#7821 = ORIENTED_EDGE ( 'NONE', *, *, #3739, .T. ) ;
#7822 = DIRECTION ( 'NONE',  ( 0.9999998435093852001, 1.040231503251046532E-15, -0.0005594472316432180879 ) ) ;
#7823 = CARTESIAN_POINT ( 'NONE',  ( 3.791570905984167794, 1.365923996832131609E-16, 0.7997593710750563467 ) ) ;
#7824 = CIRCLE ( 'NONE', #1762, 0.3625000000000019318 ) ;
#7825 = PERSON_AND_ORGANIZATION ( #7862, #8117 ) ;
#7826 = ORIENTED_EDGE ( 'NONE', *, *, #6650, .F. ) ;
#7827 = AXIS2_PLACEMENT_3D ( 'NONE', #4737, #7132, #6646 ) ;
#7828 = CARTESIAN_POINT ( 'NONE',  ( -0.001186137648316157355, 2.637500537863615158, -5.108750000000001457 ) ) ;
#7829 = CARTESIAN_POINT ( 'NONE',  ( -1.187500000000000222, 7.436775080912088498, 4.083473622047245399 ) ) ;
#7830 = FACE_OUTER_BOUND ( 'NONE', #1672, .T. ) ;
#7831 = CARTESIAN_POINT ( 'NONE',  ( 2.750000000000000444, 7.338999999999999524, 3.471636850393701401 ) ) ;
#7832 = EDGE_CURVE ( 'NONE', #7102, #5031, #7110, .T. ) ;
#7833 = FACE_OUTER_BOUND ( 'NONE', #2244, .T. ) ;
#7834 = ORIENTED_EDGE ( 'NONE', *, *, #7480, .F. ) ;
#7835 = PERSON_AND_ORGANIZATION ( #7862, #8117 ) ;
#7836 = EDGE_LOOP ( 'NONE', ( #2240, #7064, #5046, #8122 ) ) ;
#7837 = EDGE_CURVE ( 'NONE', #3103, #1901, #1097, .T. ) ;
#7838 = AXIS2_PLACEMENT_3D ( 'NONE', #6997, #682, #764 ) ;
#7839 = AXIS2_PLACEMENT_3D ( 'NONE', #5917, #884, #306 ) ;
#7840 = AXIS2_PLACEMENT_3D ( 'NONE', #1559, #1439, #7773 ) ;
#7841 = CARTESIAN_POINT ( 'NONE',  ( 2.750000000000000444, 7.964000000000000412, 4.313750000000002416 ) ) ;
#7842 = CARTESIAN_POINT ( 'NONE',  ( 0.000000000000000000, 5.113999999999999879, 0.000000000000000000 ) ) ;
#7843 = DIRECTION ( 'NONE',  ( -0.9925485533740563415, 0.000000000000000000, -0.1218497812680346959 ) ) ;
#7844 = CARTESIAN_POINT ( 'NONE',  ( 3.987953385826772390, 4.020876854703599790, 8.414523909741193464 ) ) ;
#7845 = ORIENTED_EDGE ( 'NONE', *, *, #2768, .F. ) ;
#7846 = AXIS2_PLACEMENT_3D ( 'NONE', #1184, #1761, #6180 ) ;
#7847 = APPLICATION_CONTEXT ( 'configuration controlled 3d designs of mechanical parts and assemblies' ) ;
#7848 = AXIS2_PLACEMENT_3D ( 'NONE', #4026, #4683, #3086 ) ;
#7849 = ADVANCED_FACE ( 'NONE', ( #4678 ), #7952, .T. ) ;
#7850 = CARTESIAN_POINT ( 'NONE',  ( -3.987046614173229475, 4.142615650101483027, 8.192364704391877694 ) ) ;
#7851 = CARTESIAN_POINT ( 'NONE',  ( 2.537499998660271761, 3.550000000000001155, 2.790532913385826763 ) ) ;
#7852 = CARTESIAN_POINT ( 'NONE',  ( 2.740000000000000657, 0.000000000000000000, 3.323750000000001759 ) ) ;
#7853 = PLANE ( 'NONE',  #6752 ) ;
#7854 = CARTESIAN_POINT ( 'NONE',  ( -8.751021560936518753E-10, 1.365923996832131609E-16, 5.750408897959578548E-10 ) ) ;
#7855 = AXIS2_PLACEMENT_3D ( 'NONE', #3905, #3351, #2160 ) ;
#7856 = CIRCLE ( 'NONE', #621, 1.591000000000001080 ) ;
#7857 = APPROVAL_DATE_TIME ( #1709, #6376 ) ;
#7858 = CARTESIAN_POINT ( 'NONE',  ( 1.187500000000000222, 4.160767401574803515, 6.858307716535433585 ) ) ;
#7859 = CALENDAR_DATE ( 2026, 8, 10 ) ;
#7860 = CARTESIAN_POINT ( 'NONE',  ( 0.6820189411826721448, 4.262011897367396607, 8.210925237484662631 ) ) ;
#7861 = ORIENTED_EDGE ( 'NONE', *, *, #1245, .T. ) ;
#7862 = PERSON ( 'UNSPECIFIED', 'UNSPECIFIED', 'UNSPECIFIED', ('UNSPECIFIED'), ('UNSPECIFIED'), ('UNSPECIFIED') ) ;
#7863 = DIRECTION ( 'NONE',  ( 0.000000000000000000, -0.000000000000000000, -1.000000000000000000 ) ) ;
#7864 = MANIFOLD_SOLID_BREP ( 'Imported1', #2297 ) ;
#7865 = CARTESIAN_POINT ( 'NONE',  ( -2.745000000000000995, 8.719000000000002970, 4.318750000000002309 ) ) ;
#7866 = VERTEX_POINT ( 'NONE', #6501 ) ;
#7867 = DIRECTION ( 'NONE',  ( 0.7071067811865475727, 0.7071067811865475727, 0.000000000000000000 ) ) ;
#7868 = VERTEX_POINT ( 'NONE', #7068 ) ;
#7869 = DIRECTION ( 'NONE',  ( 0.000000000000000000, 0.000000000000000000, 1.000000000000000000 ) ) ;
#7870 = CYLINDRICAL_SURFACE ( 'NONE', #6349, 4.805751768934915624 ) ;
#7871 = APPROVAL_DATE_TIME ( #6482, #7709 ) ;
#7872 = EDGE_CURVE ( 'NONE', #1434, #5017, #8183, .T. ) ;
#7873 = ORIENTED_EDGE ( 'NONE', *, *, #2836, .T. ) ;
#7874 = CARTESIAN_POINT ( 'NONE',  ( -0.1740164513111777667, 2.648365384722445093, -5.108749999999999680 ) ) ;
#7875 = CARTESIAN_POINT ( 'NONE',  ( -0.1316627106748616272, 2.329054901387897836, 3.076208900215326114 ) ) ;
#7876 = CC_DESIGN_PERSON_AND_ORGANIZATION_ASSIGNMENT ( #1015, #2886, ( #7978 ) ) ;
#7877 = CARTESIAN_POINT ( 'NONE',  ( -1.312500000000000444, 7.352492874015749358, 3.316250000000001474 ) ) ;
#7878 = LENGTH_MEASURE_WITH_UNIT ( LENGTH_MEASURE( 0.02539999999999999897 ), #4592 );
#7879 = B_SPLINE_CURVE_WITH_KNOTS ( 'NONE', 3,
 ( #2506, #6883, #1278, #2000, #7700, #7055, #6355, #2665, #20, #68, #5035, #7575, #3880, #2546, #6393, #779, #2584, #1966, #3274, #1475, #4499, #1926 ),
 .UNSPECIFIED., .F., .F.,
 ( 4, 2, 2, 2, 2, 2, 2, 2, 2, 2, 4 ),
 ( 1.465475848683458973E-11, 0.002333053235454138254, 0.004666106456253518199, 0.009332212897852278088, 0.01399831933945103885, 0.01866442578104979960, 0.02799663866424725867, 0.03732885154744471773, 0.04666106443064217679, 0.05599327731383962892, 0.07465770308023454704 ),
 .UNSPECIFIED. ) ;
#7880 = PERSON_AND_ORGANIZATION_ROLE ( 'classification_officer' ) ;
#7881 = ORIENTED_EDGE ( 'NONE', *, *, #6447, .T. ) ;
#7882 = DIRECTION ( 'NONE',  ( 0.000000000000000000, 0.7071067811865474617, 0.7071067811865474617 ) ) ;
#7883 = EDGE_CURVE ( 'NONE', #1240, #7297, #6587, .T. ) ;
#7884 = UNCERTAINTY_MEASURE_WITH_UNIT (LENGTH_MEASURE( 1.000000000000000082E-05 ), #4708, 'distance_accuracy_value', 'NONE');
#7885 = EDGE_CURVE ( 'NONE', #3887, #1328, #5287, .T. ) ;
#7886 = CARTESIAN_POINT ( 'NONE',  ( -0.7499999999999993339, 3.950000000000000178, 7.231250000000000178 ) ) ;
#7887 = DIRECTION ( 'NONE',  ( 1.000000000000000000, 0.000000000000000000, 0.000000000000000000 ) ) ;
#7888 = ORIENTED_EDGE ( 'NONE', *, *, #1584, .F. ) ;
#7889 = DIRECTION ( 'NONE',  ( -0.000000000000000000, -0.000000000000000000, 1.000000000000000000 ) ) ;
#7890 = ORIENTED_EDGE ( 'NONE', *, *, #2991, .F. ) ;
#7891 = CARTESIAN_POINT ( 'NONE',  ( -1.644500000000000739, 2.305500000000000771, -5.108750000000001457 ) ) ;
#7892 = CARTESIAN_POINT ( 'NONE',  ( -8.751021560936518753E-10, 1.365923996832131609E-16, 5.750408897959578548E-10 ) ) ;
#7893 = CARTESIAN_POINT ( 'NONE',  ( 2.750000000000000444, 8.729000000000002757, 3.833750000000001545 ) ) ;
#7894 = FACE_OUTER_BOUND ( 'NONE', #3517, .T. ) ;
#7895 = ORIENTED_EDGE ( 'NONE', *, *, #7587, .F. ) ;
#7896 = COORDINATED_UNIVERSAL_TIME_OFFSET ( 0, 0, .AHEAD. ) ;
#7897 = CARTESIAN_POINT ( 'NONE',  ( 0.000000000000000000, 0.000000000000000000, 3.323750000000001759 ) ) ;
#7898 = EDGE_CURVE ( 'NONE', #3927, #2985, #2800, .T. ) ;
#7899 = CARTESIAN_POINT ( 'NONE',  ( 0.7077600209949282961, 4.198434470451293699, 8.040603848493715233 ) ) ;
#7900 = ORIENTED_EDGE ( 'NONE', *, *, #6093, .F. ) ;
#7901 = DIRECTION ( 'NONE',  ( -0.000000000000000000, -0.000000000000000000, -1.000000000000000000 ) ) ;
#7902 = LOCAL_TIME ( 0, 37, 23.00000000000000000, #4122 ) ;
#7903 = ORIENTED_EDGE ( 'NONE', *, *, #8114, .F. ) ;
#7904 = DIRECTION ( 'NONE',  ( -0.000000000000000000, 0.000000000000000000, 1.000000000000000000 ) ) ;
#7905 = CARTESIAN_POINT ( 'NONE',  ( -0.7499999999999993339, 3.950000000000000178, 7.231250000000000178 ) ) ;
#7906 = ORIENTED_EDGE ( 'NONE', *, *, #7781, .F. ) ;
#7907 = PERSON_AND_ORGANIZATION_ROLE ( 'creator' ) ;
#7908 = DIRECTION ( 'NONE',  ( -0.000000000000000000, 1.000000000000000000, 0.000000000000000000 ) ) ;
#7909 = SHAPE_DEFINITION_REPRESENTATION ( #6474, #4813 ) ;
#7910 = EDGE_CURVE ( 'NONE', #6912, #6003, #4093, .T. ) ;
#7911 = ORIENTED_EDGE ( 'NONE', *, *, #2928, .T. ) ;
#7912 = CARTESIAN_POINT ( 'NONE',  ( -2.750000000000000444, 7.964000000000001300, 3.691250000000001030 ) ) ;
#7913 = CARTESIAN_POINT ( 'NONE',  ( -1.277972681119055709, 4.249847095080741433, -5.108750000000003233 ) ) ;
#7914 = CARTESIAN_POINT ( 'NONE',  ( -0.7335700375402988138, 2.499999999992026378, 2.908930215739981229 ) ) ;
#7915 = FACE_OUTER_BOUND ( 'NONE', #6713, .T. ) ;
#7916 = CARTESIAN_POINT ( 'NONE',  ( 3.583510604133040900, 1.543025754838326824, 7.167021208266081800 ) ) ;
#7917 = CALENDAR_DATE ( 2026, 8, 10 ) ;
#7918 = ORIENTED_EDGE ( 'NONE', *, *, #7883, .F. ) ;
#7919 = DIRECTION ( 'NONE',  ( -0.000000000000000000, -0.7071067811865474617, 0.7071067811865474617 ) ) ;
#7920 = CC_DESIGN_PERSON_AND_ORGANIZATION_ASSIGNMENT ( #3276, #3196, ( #6809 ) ) ;
#7921 = EDGE_CURVE ( 'NONE', #7136, #1059, #5877, .T. ) ;
#7922 = FACE_OUTER_BOUND ( 'NONE', #7534, .T. ) ;
#7923 = DIRECTION ( 'NONE',  ( 0.000000000000000000, 1.000000000000000000, -0.000000000000000000 ) ) ;
#7924 = CARTESIAN_POINT ( 'NONE',  ( -2.537500000000000533, 2.500000000000000444, -0.2625000000000008438 ) ) ;
#7925 = VERTEX_POINT ( 'NONE', #4599 ) ;
#7926 = CARTESIAN_POINT ( 'NONE',  ( -3.987046614173229919, 4.051924899701968563, 8.063218304145049586 ) ) ;
#7927 = LINE ( 'NONE', #1703, #744 ) ;
#7928 = EDGE_CURVE ( 'NONE', #3049, #6239, #1467, .T. ) ;
#7929 = EDGE_CURVE ( 'NONE', #5413, #3502, #2879, .T. ) ;
#7930 = CARTESIAN_POINT ( 'NONE',  ( 0.000000000000000000, 2.875000000000000888, 3.742515787401575533 ) ) ;
#7931 = LINE ( 'NONE', #6634, #3709 ) ;
#7932 = DIRECTION ( 'NONE',  ( 0.000000000000000000, 1.000000000000000000, 0.000000000000000000 ) ) ;
#7933 = EDGE_LOOP ( 'NONE', ( #248, #5555, #1985, #5654 ) ) ;
#7934 = DATE_TIME_ROLE ( 'creation_date' ) ;
#7935 = DIRECTION ( 'NONE',  ( 0.000000000000000000, 0.000000000000000000, -1.000000000000000000 ) ) ;
#7936 = AXIS2_PLACEMENT_3D ( 'NONE', #5567, #7451, #3798 ) ;
#7937 = CARTESIAN_POINT ( 'NONE',  ( 0.7314405957411594938, 4.116041651862893502, 7.966316554334127886 ) ) ;
#7938 = EDGE_CURVE ( 'NONE', #2826, #4397, #1044, .T. ) ;
#7939 = LOCAL_TIME ( 0, 37, 23.00000000000000000, #5600 ) ;
#7940 = ORIENTED_EDGE ( 'NONE', *, *, #113, .F. ) ;
#7941 = VECTOR ( 'NONE', #7795, 39.37007874015748143 ) ;
#7942 = AXIS2_PLACEMENT_3D ( 'NONE', #7124, #2770, #5182 ) ;
#7943 = ORIENTED_EDGE ( 'NONE', *, *, #7373, .T. ) ;
#7944 = CARTESIAN_POINT ( 'NONE',  ( -4.462046614173230452, 4.225666661560478765, 7.679916707260899145 ) ) ;
#7945 = CARTESIAN_POINT ( 'NONE',  ( 2.750000000000000888, 7.974000000000001087, 3.333750000000001990 ) ) ;
#7946 = ORIENTED_EDGE ( 'NONE', *, *, #6152, .F. ) ;
#7947 = DATE_TIME_ROLE ( 'creation_date' ) ;
#7948 = DIRECTION ( 'NONE',  ( 0.000000000000000000, -0.7071067811865474617, -0.7071067811865474617 ) ) ;
#7949 = CALENDAR_DATE ( 2026, 8, 10 ) ;
#7950 = EDGE_LOOP ( 'NONE', ( #5730, #5238 ) ) ;
#7951 = EDGE_CURVE ( 'NONE', #3948, #3578, #5492, .T. ) ;
#7952 =( BOUNDED_SURFACE ( )  B_SPLINE_SURFACE ( 3, 3, ( 
 ( #915, #3416, #2191, #1574 ),
 ( #3976, #829, #5910, #338 ),
 ( #3455, #3332, #298, #2720 ),
 ( #4055, #4639, #4019, #218 ),
 ( #5244, #2107, #7233, #5837 ),
 ( #3373, #6546, #5209, #1496 ) ),
 .UNSPECIFIED., .F., .F., .T. ) 
 B_SPLINE_SURFACE_WITH_KNOTS ( ( 4, 2, 4 ),
 ( 4, 4 ),
 ( 0.000000000000000000, 0.5000000000000000000, 1.000000000000000000 ),
 ( 0.000000000000000000, 1.000000000000000000 ),
 .UNSPECIFIED. ) 
 GEOMETRIC_REPRESENTATION_ITEM ( )  RATIONAL_B_SPLINE_SURFACE ( (
 ( 1.000000000000000000, 0.3333333333333334259, 0.3333333333333334259, 1.000000000000000000),
 ( 1.000000000000000000, 0.3333333333333334259, 0.3333333333333334259, 1.000000000000000000),
 ( 1.000000000000000000, 0.3333333333333334259, 0.3333333333333334259, 1.000000000000000000),
 ( 1.000000000000000000, 0.3333333333333334259, 0.3333333333333334259, 1.000000000000000000),
 ( 1.000000000000000000, 0.3333333333333334259, 0.3333333333333334259, 1.000000000000000000),
 ( 1.000000000000000000, 0.3333333333333334259, 0.3333333333333334259, 1.000000000000000000) ) ) 
 REPRESENTATION_ITEM ( '' )  SURFACE ( )  );
#7953 = ADVANCED_BREP_SHAPE_REPRESENTATION ( '', ( #2701, #7272 ), #456 ) ;
#7954 = VECTOR ( 'NONE', #5909, 39.37007874015748854 ) ;
#7955 = DIRECTION ( 'NONE',  ( 0.000000000000000000, 0.000000000000000000, -1.000000000000000000 ) ) ;
#7956 = FACE_OUTER_BOUND ( 'NONE', #3284, .T. ) ;
#7957 = VECTOR ( 'NONE', #4308, 39.37007874015748143 ) ;
#7958 = LENGTH_MEASURE_WITH_UNIT ( LENGTH_MEASURE( 0.02539999999999999897 ), #6723 );
#7959 = DIRECTION ( 'NONE',  ( 1.000000000000000000, 1.524752368556799034E-15, 0.000000000000000000 ) ) ;
#7960 = AXIS2_PLACEMENT_3D ( 'NONE', #5746, #7504, #1890 ) ;
#7961 = COORDINATED_UNIVERSAL_TIME_OFFSET ( 0, 0, .AHEAD. ) ;
#7962 = ORIENTED_EDGE ( 'NONE', *, *, #4323, .F. ) ;
#7963 = CARTESIAN_POINT ( 'NONE',  ( -3.583510604133041344, 1.543025754838327046, 4.388534791062126923E-16 ) ) ;
#7964 = CARTESIAN_POINT ( 'NONE',  ( 2.750000000000000888, 8.719000000000001194, 3.813750000000002416 ) ) ;
#7965 = VECTOR ( 'NONE', #2415, 39.37007874015748143 ) ;
#7966 = DESIGN_CONTEXT ( 'detailed design', #6024, 'design' ) ;
#7967 = VECTOR ( 'NONE', #7308, 39.37007874015748143 ) ;
#7968 = APPROVAL ( #6176, 'UNKNOWN' ) ;
#7969 = PLANE ( 'NONE',  #1889 ) ;
#7970 = AXIS2_PLACEMENT_3D ( 'NONE', #186, #1338, #3868 ) ;
#7971 = DIRECTION ( 'NONE',  ( 0.000000000000000000, 1.000000000000000000, 0.000000000000000000 ) ) ;
#7972 = CARTESIAN_POINT ( 'NONE',  ( 2.875000000000000888, 1.000000000000000222, -2.975000000000000977 ) ) ;
#7973 = VECTOR ( 'NONE', #796, 39.37007874015748143 ) ;
#7974 = FACE_OUTER_BOUND ( 'NONE', #6257, .T. ) ;
#7975 = ORIENTED_EDGE ( 'NONE', *, *, #2205, .T. ) ;
#7976 = CARTESIAN_POINT ( 'NONE',  ( -3.987046614173228587, 4.054690900397527109, 8.064926832397588896 ) ) ;
#7977 = DIRECTION ( 'NONE',  ( -1.000000000000000000, -0.000000000000000000, -0.000000000000000000 ) ) ;
#7978 = PRODUCT_DEFINITION ( 'UNKNOWN', '', #303, #7106 ) ;
#7979 = DIRECTION ( 'NONE',  ( 0.000000000000000000, 0.000000000000000000, -1.000000000000000000 ) ) ;
#7980 = DIRECTION ( 'NONE',  ( 0.000000000000000000, -0.000000000000000000, 1.000000000000000000 ) ) ;
#7981 = VERTEX_POINT ( 'NONE', #4139 ) ;
#7982 = PERSON_AND_ORGANIZATION_ROLE ( 'design_supplier' ) ;
#7983 = DIRECTION ( 'NONE',  ( -1.000000000000000000, 0.000000000000000000, -0.000000000000000000 ) ) ;
#7984 = VECTOR ( 'NONE', #7459, 39.37007874015748854 ) ;
#7985 = CIRCLE ( 'NONE', #7707, 0.3625000012227142521 ) ;
#7986 = DIRECTION ( 'NONE',  ( 0.000000000000000000, 0.000000000000000000, 1.000000000000000000 ) ) ;
#7987 = EDGE_CURVE ( 'NONE', #963, #6692, #2912, .T. ) ;
#7988 = ORIENTED_EDGE ( 'NONE', *, *, #7153, .F. ) ;
#7989 = VECTOR ( 'NONE', #4493, 39.37007874015748143 ) ;
#7990 = CARTESIAN_POINT ( 'NONE',  ( 0.000000000000000000, 2.359000000000000874, 3.956250000000000266 ) ) ;
#7991 = CIRCLE ( 'NONE', #6893, 5.349138356872925826 ) ;
#7992 = EDGE_CURVE ( 'NONE', #5154, #2528, #2409, .T. ) ;
#7993 = ORIENTED_EDGE ( 'NONE', *, *, #2525, .F. ) ;
#7994 = CARTESIAN_POINT ( 'NONE',  ( -4.462046614173230452, 3.674333370316265057, 7.679916707260899145 ) ) ;
#7995 = ORIENTED_EDGE ( 'NONE', *, *, #4125, .T. ) ;
#7996 = PERSON_AND_ORGANIZATION ( #7862, #8117 ) ;
#7997 = DIRECTION ( 'NONE',  ( 0.000000000000000000, 0.000000000000000000, -1.000000000000000000 ) ) ;
#7998 = CARTESIAN_POINT ( 'NONE',  ( 2.875000000000000888, 1.000000000000000222, -2.975000000000000977 ) ) ;
#7999 = CALENDAR_DATE ( 2026, 8, 10 ) ;
#8000 = ORIENTED_EDGE ( 'NONE', *, *, #2991, .T. ) ;
#8001 = DIRECTION ( 'NONE',  ( -0.000000000000000000, -1.000000000000000000, -0.000000000000000000 ) ) ;
#8002 = CIRCLE ( 'NONE', #2321, 3.000000000000000888 ) ;
#8003 = AXIS2_PLACEMENT_3D ( 'NONE', #2755, #7790, #2795 ) ;
#8004 = CARTESIAN_POINT ( 'NONE',  ( -1.889618362131626726E-10, 5.113999999999999879, 2.750000000234376074 ) ) ;
#8005 = CARTESIAN_POINT ( 'NONE',  ( 0.4152326938056751793, 2.378623393394907026, 3.027452056815282955 ) ) ;
#8006 = CARTESIAN_POINT ( 'NONE',  ( -0.6907419235105254351, 4.242221832517436120, 8.120048698298123924 ) ) ;
#8007 = AXIS2_PLACEMENT_3D ( 'NONE', #2431, #6271, #658 ) ;
#8008 = DIRECTION ( 'NONE',  ( 0.000000000000000000, 0.000000000000000000, -1.000000000000000000 ) ) ;
#8009 = APPROVAL_ROLE ( '' ) ;
#8010 = EDGE_LOOP ( 'NONE', ( #4733, #3748, #7529, #6642, #2492 ) ) ;
#8011 = EDGE_CURVE ( 'NONE', #266, #4928, #3032, .T. ) ;
#8012 = EDGE_CURVE ( 'NONE', #4355, #1456, #1196, .T. ) ;
#8013 = DIRECTION ( 'NONE',  ( -0.000000000000000000, 1.000000000000000000, 0.000000000000000000 ) ) ;
#8014 = CARTESIAN_POINT ( 'NONE',  ( -1.500000000000000444, 5.113999999999999879, 0.1249999999999999029 ) ) ;
#8015 = DIRECTION ( 'NONE',  ( 0.7071067811865554553, -1.583668658704876446E-14, -0.7071067811865395791 ) ) ;
#8016 = EDGE_CURVE ( 'NONE', #2186, #295, #5551, .T. ) ;
#8017 = CARTESIAN_POINT ( 'NONE',  ( -3.651126736336024248, 1.000000000000000444, -1.298036422402331302 ) ) ;
#8018 = VERTEX_POINT ( 'NONE', #3087 ) ;
#8019 = DIRECTION ( 'NONE',  ( -0.7071067811865474617, 0.7071067811865474617, 0.000000000000000000 ) ) ;
#8020 = ORIENTED_EDGE ( 'NONE', *, *, #7196, .T. ) ;
#8021 = CARTESIAN_POINT ( 'NONE',  ( -3.296097361031207207, 1.750000000037170489, -0.5624999991015005030 ) ) ;
#8022 = LINE ( 'NONE', #3095, #3961 ) ;
#8023 = DIRECTION ( 'NONE',  ( 0.000000000000000000, 0.000000000000000000, -1.000000000000000000 ) ) ;
#8024 = VERTEX_POINT ( 'NONE', #1777 ) ;
#8025 = PERSON_AND_ORGANIZATION_ROLE ( 'design_owner' ) ;
#8026 = DIRECTION ( 'NONE',  ( -0.000000000000000000, -0.000000000000000000, 1.000000000000000000 ) ) ;
#8027 = CC_DESIGN_PERSON_AND_ORGANIZATION_ASSIGNMENT ( #4919, #1726, ( #3413 ) ) ;
#8028 = EDGE_LOOP ( 'NONE', ( #6130, #7834, #4735, #7512 ) ) ;
#8029 = DIRECTION ( 'NONE',  ( 0.000000000000000000, 0.000000000000000000, 1.000000000000000000 ) ) ;
#8030 = EDGE_CURVE ( 'NONE', #7789, #7058, #3596, .T. ) ;
#8031 = CARTESIAN_POINT ( 'NONE',  ( 2.740000000000001545, 7.964000000000000412, 4.313750000000002416 ) ) ;
#8032 = DIRECTION ( 'NONE',  ( -1.000000000000000000, 0.000000000000000000, 0.000000000000000000 ) ) ;
#8033 = ORIENTED_EDGE ( 'NONE', *, *, #731, .F. ) ;
#8034 = PERSON_AND_ORGANIZATION ( #7862, #8117 ) ;
#8035 = DIRECTION ( 'NONE',  ( 0.000000000000000000, 0.000000000000000000, 1.000000000000000000 ) ) ;
#8036 = FACE_OUTER_BOUND ( 'NONE', #1831, .T. ) ;
#8037 = CARTESIAN_POINT ( 'NONE',  ( -0.7499999999999993339, 3.950000000000000622, 8.543750000000002842 ) ) ;
#8038 = APPROVAL_STATUS ( 'not_yet_approved' ) ;
#8039 = PRODUCT_DEFINITION_SHAPE ( 'NONE', 'NONE',  #5310 ) ;
#8040 = EDGE_CURVE ( 'NONE', #7672, #5894, #5913, .T. ) ;
#8041 = ORGANIZATION ( 'NAUO-ORG3', 'UNSPECIFIED', 'UNSPECIFIED' ) ;
#8042 = DIRECTION ( 'NONE',  ( -1.000000000000000000, 0.000000000000000000, -0.000000000000000000 ) ) ;
#8043 = DIRECTION ( 'NONE',  ( -0.000000000000000000, 0.000000000000000000, 1.000000000000000000 ) ) ;
#8044 = EDGE_CURVE ( 'NONE', #5792, #2504, #717, .T. ) ;
#8045 = VERTEX_POINT ( 'NONE', #1732 ) ;
#8046 = CARTESIAN_POINT ( 'NONE',  ( -0.6820189411826721448, 4.262011897367396607, 8.251574762515335948 ) ) ;
#8047 = LOCAL_TIME ( 0, 37, 23.00000000000000000, #5218 ) ;
#8048 = CARTESIAN_POINT ( 'NONE',  ( -3.362500000000001155, 1.750000000000000444, 4.117874862132976456E-16 ) ) ;
#8049 = DATE_AND_TIME ( #4171, #3011 ) ;
#8050 = ORIENTED_EDGE ( 'NONE', *, *, #7004, .F. ) ;
#8051 = CARTESIAN_POINT ( 'NONE',  ( -3.362500000000002931, 1.750000000000000222, -6.725000000000002309 ) ) ;
#8052 = EDGE_CURVE ( 'NONE', #3578, #6815, #1115, .T. ) ;
#8053 = EDGE_LOOP ( 'NONE', ( #1892, #2049, #5819, #7995, #2805 ) ) ;
#8054 = DIRECTION ( 'NONE',  ( 1.000000000000000000, 0.000000000000000000, 0.000000000000000000 ) ) ;
#8055 = CARTESIAN_POINT ( 'NONE',  ( -2.537500000000000533, 2.500000000000000444, -0.000000000000000000 ) ) ;
#8056 = CARTESIAN_POINT ( 'NONE',  ( -2.745000000000000995, 7.974000000000001087, 3.328750000000002096 ) ) ;
#8057 = ORIENTED_EDGE ( 'NONE', *, *, #7992, .F. ) ;
#8058 = DIRECTION ( 'NONE',  ( -0.7071067811865474617, 0.000000000000000000, 0.7071067811865474617 ) ) ;
#8059 = CARTESIAN_POINT ( 'NONE',  ( -0.6907419235105256572, 3.657778167482562459, 8.342451301701874655 ) ) ;
#8060 = ORIENTED_EDGE ( 'NONE', *, *, #5697, .F. ) ;
#8061 = CARTESIAN_POINT ( 'NONE',  ( 3.987953385826771946, 4.107055349781281173, 8.112380013460960271 ) ) ;
#8062 = ADVANCED_FACE ( 'NONE', ( #2994, #3695 ), #7969, .F. ) ;
#8063 = CARTESIAN_POINT ( 'NONE',  ( -1.356031417322835608, 5.217694212598425807, -5.293171771653544688 ) ) ;
#8064 = FACE_OUTER_BOUND ( 'NONE', #1769, .T. ) ;
#8065 = DIRECTION ( 'NONE',  ( 0.000000000000000000, -1.000000000000000000, 0.000000000000000000 ) ) ;
#8066 = ORIENTED_EDGE ( 'NONE', *, *, #5998, .T. ) ;
#8067 = PERSON_AND_ORGANIZATION_ROLE ( 'creator' ) ;
#8068 = CARTESIAN_POINT ( 'NONE',  ( -2.740000000000000657, 7.964000000000000412, 3.813750000000002416 ) ) ;
#8069 = ORIENTED_EDGE ( 'NONE', *, *, #2395, .F. ) ;
#8070 = CARTESIAN_POINT ( 'NONE',  ( 2.750000000000000000, 7.521783347043602852, 3.691250000474206150 ) ) ;
#8071 = FACE_OUTER_BOUND ( 'NONE', #5002, .T. ) ;
#8072 = DIRECTION ( 'NONE',  ( -0.000000000000000000, -1.000000000000000000, -0.000000000000000000 ) ) ;
#8073 = ORIENTED_EDGE ( 'NONE', *, *, #3582, .F. ) ;
#8074 = MECHANICAL_CONTEXT ( 'NONE', #4444, 'mechanical' ) ;
#8075 = APPROVAL ( #4829, 'UNKNOWN' ) ;
#8076 = DIRECTION ( 'NONE',  ( -1.000000000000000000, 0.000000000000000000, 0.000000000000000000 ) ) ;
#8077 = LOCAL_TIME ( 0, 37, 23.00000000000000000, #6174 ) ;
#8078 = DATE_TIME_ROLE ( 'classification_date' ) ;
#8079 = EDGE_CURVE ( 'NONE', #7925, #1840, #537, .T. ) ;
#8080 = VECTOR ( 'NONE', #8058, 39.37007874015748854 ) ;
#8081 = AXIS2_PLACEMENT_3D ( 'NONE', #3794, #7642, #729 ) ;
#8082 = CC_DESIGN_APPROVAL ( #2421, ( #5310 ) ) ;
#8083 = CARTESIAN_POINT ( 'NONE',  ( 1.172489671196043304, 1.000000000000000444, -3.693357952326151494 ) ) ;
#8084 = CARTESIAN_POINT ( 'NONE',  ( 2.740000000000001545, 8.724000000000001975, 4.318750000000002309 ) ) ;
#8085 = DIRECTION ( 'NONE',  ( 0.000000000000000000, 0.000000000000000000, -1.000000000000000000 ) ) ;
#8086 = VERTEX_POINT ( 'NONE', #5532 ) ;
#8087 = CARTESIAN_POINT ( 'NONE',  ( -0.7386972477860228592, 4.080064161770346587, 8.515578956946558975 ) ) ;
#8088 =( NAMED_UNIT ( * ) PLANE_ANGLE_UNIT ( ) SI_UNIT ( $, .RADIAN. ) );
#8089 = APPROVAL ( #1300, 'UNSPECIFIED' ) ;
#8090 = CARTESIAN_POINT ( 'NONE',  ( 2.637478091534485092, 0.9999999999988804511, -2.843572666449059927 ) ) ;
#8091 = APPROVAL_STATUS ( 'not_yet_approved' ) ;
#8092 = VERTEX_POINT ( 'NONE', #6119 ) ;
#8093 = CIRCLE ( 'NONE', #7265, 0.2625000000000008438 ) ;
#8094 = CYLINDRICAL_SURFACE ( 'NONE', #6247, 1.124999999999999556 ) ;
#8095 = ADVANCED_FACE ( 'NONE', ( #2436 ), #7329, .T. ) ;
#8096 = AXIS2_PLACEMENT_3D ( 'NONE', #3041, #7979, #8110 ) ;
#8097 = EDGE_LOOP ( 'NONE', ( #910, #1588, #3524, #3968, #7439, #7918, #3925, #2821, #6936 ) ) ;
#8098 = EDGE_CURVE ( 'NONE', #1286, #1721, #1767, .T. ) ;
#8099 = AXIS2_PLACEMENT_3D ( 'NONE', #4463, #5824, #207 ) ;
#8100 = LINE ( 'NONE', #1731, #6335 ) ;
#8101 = CARTESIAN_POINT ( 'NONE',  ( 2.749999999999999556, 7.339000000000001300, 4.486250000000000959 ) ) ;
#8102 = EDGE_CURVE ( 'NONE', #6859, #7256, #7621, .T. ) ;
#8103 = EDGE_LOOP ( 'NONE', ( #2514, #4845 ) ) ;
#8104 = CARTESIAN_POINT ( 'NONE',  ( -0.6854931847115989241, 3.645690833133080400, 8.303072425453409622 ) ) ;
#8105 = ORIENTED_EDGE ( 'NONE', *, *, #6551, .F. ) ;
#8106 = AXIS2_PLACEMENT_3D ( 'NONE', #3194, #5691, #1560 ) ;
#8107 = CARTESIAN_POINT ( 'NONE',  ( 3.987953385826774166, 4.063153587258190313, 8.070563664178681762 ) ) ;
#8108 = CYLINDRICAL_SURFACE ( 'NONE', #6459, 1.074999999999999289 ) ;
#8109 = PRODUCT ( 'bench vise8-', 'bench vise8-', '', ( #607 ) ) ;
#8110 = DIRECTION ( 'NONE',  ( 1.000000000000000000, -1.681137231067760553E-15, 0.000000000000000000 ) ) ;
#8111 = ORIENTED_EDGE ( 'NONE', *, *, #3833, .T. ) ;
#8112 = PERSON_AND_ORGANIZATION_ROLE ( 'design_supplier' ) ;
#8113 = DIRECTION ( 'NONE',  ( 0.000000000000000000, 0.000000000000000000, 1.000000000000000000 ) ) ;
#8114 = EDGE_CURVE ( 'NONE', #4495, #6784, #3808, .T. ) ;
#8115 = ADVANCED_FACE ( 'NONE', ( #7542 ), #6318, .T. ) ;
#8116 = AXIS2_PLACEMENT_3D ( 'NONE', #2451, #3079, #1856 ) ;
#8117 = ORGANIZATION ( 'UNSPECIFIED', 'UNSPECIFIED', '' ) ;
#8118 = ORIENTED_EDGE ( 'NONE', *, *, #2634, .F. ) ;
#8119 = FACE_OUTER_BOUND ( 'NONE', #2823, .T. ) ;
#8120 = LINE ( 'NONE', #2460, #1374 ) ;
#8121 = FACE_OUTER_BOUND ( 'NONE', #5881, .T. ) ;
#8122 = ORIENTED_EDGE ( 'NONE', *, *, #2537, .T. ) ;
#8123 = APPROVAL_ROLE ( '' ) ;
#8124 = CARTESIAN_POINT ( 'NONE',  ( 4.067120052493439886, 4.383999996532200072, 8.231249998505111520 ) ) ;
#8125 = APPROVAL_DATE_TIME ( #3058, #5208 ) ;
#8126 = AXIS2_PLACEMENT_3D ( 'NONE', #2045, #3909, #807 ) ;
#8127 = CIRCLE ( 'NONE', #4528, 0.6000000000000015321 ) ;
#8128 = FACE_OUTER_BOUND ( 'NONE', #5338, .T. ) ;
#8129 = PLANE ( 'NONE',  #2184 ) ;
#8130 = CARTESIAN_POINT ( 'NONE',  ( 3.296097360936645959, 1.749999999910763826, -0.5625000000000002220 ) ) ;
#8131 = ORIENTED_EDGE ( 'NONE', *, *, #743, .T. ) ;
#8132 = CARTESIAN_POINT ( 'NONE',  ( -0.7466433925744946354, 4.021593608141584397, 7.926888364618726257 ) ) ;
#8133 = EDGE_CURVE ( 'NONE', #7256, #4377, #5042, .T. ) ;
#8134 = LINE ( 'NONE', #4871, #191 ) ;
#8135 = SECURITY_CLASSIFICATION_LEVEL ( 'unclassified' ) ;
#8136 = ORIENTED_EDGE ( 'NONE', *, *, #1470, .F. ) ;
#8137 = PLANE ( 'NONE',  #6533 ) ;
#8138 = CC_DESIGN_DATE_AND_TIME_ASSIGNMENT ( #1690, #6656, ( #1319 ) ) ;
#8139 = VERTEX_POINT ( 'NONE', #5701 ) ;
#8140 = AXIS2_PLACEMENT_3D ( 'NONE', #6234, #5614, #4461 ) ;
#8141 = PLANE ( 'NONE',  #6467 ) ;
#8142 = CARTESIAN_POINT ( 'NONE',  ( 0.7335700379894659617, 2.500000000219264606, 2.749999999536766992 ) ) ;
#8143 = CARTESIAN_POINT ( 'NONE',  ( 4.067120052493439886, 4.383999996532200072, 8.231249998505111520 ) ) ;
#8144 = CARTESIAN_POINT ( 'NONE',  ( -1.388463899750249738E-31, 3.950000000000000178, 3.440250000000000696 ) ) ;
#8145 = ORIENTED_EDGE ( 'NONE', *, *, #6956, .F. ) ;
#8146 = VERTEX_POINT ( 'NONE', #1361 ) ;
#8147 = B_SPLINE_CURVE_WITH_KNOTS ( 'NONE', 3,
 ( #536, #5617, #6733, #1816 ),
 .UNSPECIFIED., .F., .F.,
 ( 4, 4 ),
 ( 6.031472751832138938E-13, 0.02101476597407635552 ),
 .UNSPECIFIED. ) ;
#8148 = EDGE_CURVE ( 'NONE', #7410, #5001, #3846, .T. ) ;
#8149 = CARTESIAN_POINT ( 'NONE',  ( 3.987953385826772390, 4.146499994074616779, 8.218759808174304737 ) ) ;
#8150 = CARTESIAN_POINT ( 'NONE',  ( 0.1355816141732284208, 5.291204763779528086, -5.034844055118110617 ) ) ;
#8151 = CARTESIAN_POINT ( 'NONE',  ( 1.187500000000000000, 4.446184378179288466, 6.518065150780170569 ) ) ;
#8152 = ORIENTED_EDGE ( 'NONE', *, *, #4976, .T. ) ;
#8154 = PERSON_AND_ORGANIZATION ( #7862, #8117 ) ;
#8153 = PRODUCT_DEFINITION_FORMATION_WITH_SPECIFIED_SOURCE ( 'ANY', '', #6809, .NOT_KNOWN. ) ;
#8155 = CARTESIAN_POINT ( 'NONE',  ( 3.987953385826771946, 3.765347506452387805, 8.298484949317723292 ) ) ;
#8156 = ADVANCED_FACE ( 'NONE', ( #3240 ), #76, .F. ) ;
#8157 = ORIENTED_EDGE ( 'NONE', *, *, #6890, .F. ) ;
#8158 = ADVANCED_FACE ( 'NONE', ( #703 ), #3160, .T. ) ;
#8159 = LOCAL_TIME ( 0, 37, 23.00000000000000000, #4042 ) ;
#8160 = CYLINDRICAL_SURFACE ( 'NONE', #5988, 0.3625000012227142521 ) ;
#8161 = CARTESIAN_POINT ( 'NONE',  ( 2.740000000000000657, 7.964000000000000412, 3.333750000000001990 ) ) ;
#8162 = CARTESIAN_POINT ( 'NONE',  ( 1.625000000000000222, 2.499999999434268982, 2.521780125537467665 ) ) ;
#8163 = EDGE_LOOP ( 'NONE', ( #3733, #4429 ) ) ;
#8164 = PERSON_AND_ORGANIZATION ( #7862, #8117 ) ;
#8165 = CARTESIAN_POINT ( 'NONE',  ( 3.987953385826771946, 3.753500037802128375, 8.231249998505111520 ) ) ;
#8166 = COORDINATED_UNIVERSAL_TIME_OFFSET ( 0, 0, .AHEAD. ) ;
#8167 = CARTESIAN_POINT ( 'NONE',  ( -1.624999999999998890, 5.113999999999999879, 2.749999998942535218 ) ) ;
#8168 = CARTESIAN_POINT ( 'NONE',  ( -1.198957880909643725, 2.499999999928966599, 2.750000000000000444 ) ) ;
#8169 = DIMENSIONAL_EXPONENTS ( 1.000000000000000000, 0.000000000000000000, 0.000000000000000000, 0.000000000000000000, 0.000000000000000000, 0.000000000000000000, 0.000000000000000000 ) ;
#8170 = PERSON ( 'NAUO-PER7', 'UNSPECIFIED', 'UNSPECIFIED', ('UNSPECIFIED'), ('UNSPECIFIED'), ('UNSPECIFIED') ) ;
#8171 = DIRECTION ( 'NONE',  ( 0.000000000000000000, 1.000000000000000000, 0.000000000000000000 ) ) ;
#8172 = LINE ( 'NONE', #4373, #3219 ) ;
#8173 = CARTESIAN_POINT ( 'NONE',  ( -4.462046614173229564, 3.950000015938371689, 8.231249998505111520 ) ) ;
#8174 = ORIENTED_EDGE ( 'NONE', *, *, #2731, .F. ) ;
#8175 = CARTESIAN_POINT ( 'NONE',  ( -4.462046614173230452, 4.225666661560478765, 8.782583289749325672 ) ) ;
#8176 = EDGE_CURVE ( 'NONE', #7262, #1328, #1934, .T. ) ;
#8177 =( LENGTH_UNIT ( ) NAMED_UNIT ( * ) SI_UNIT ( $, .METRE. ) );
#8178 = CARTESIAN_POINT ( 'NONE',  ( 3.343750000000002220, 1.750000000000000444, 0.5624999982029994516 ) ) ;
#8179 = MECHANICAL_CONTEXT ( 'NONE', #7793, 'mechanical' ) ;
#8180 = ORIENTED_EDGE ( 'NONE', *, *, #4977, .F. ) ;
#8181 = CARTESIAN_POINT ( 'NONE',  ( 3.479221556377631263E-16, 1.750000000000000444, -2.841000000000000636 ) ) ;
#8182 = APPLICATION_CONTEXT ( 'configuration controlled 3d designs of mechanical parts and assemblies' ) ;
#8183 =( BOUNDED_CURVE ( )  B_SPLINE_CURVE ( 3, ( #7152, #875, #5366, #7192 ),
 .UNSPECIFIED., .F., .F. ) 
 B_SPLINE_CURVE_WITH_KNOTS ( ( 4, 4 ),
 ( 0.000000000000000000, 1.000000000000000000 ),
 .UNSPECIFIED. ) 
 CURVE ( )  GEOMETRIC_REPRESENTATION_ITEM ( )  RATIONAL_B_SPLINE_CURVE ( ( 1.000000000000000000, 0.9963935896217739341, 0.9963935896217739341, 1.000000000000000000 ) ) 
 REPRESENTATION_ITEM ( '' )  );
#8184 = CARTESIAN_POINT ( 'NONE',  ( 3.987953385826771946, 4.225666661560476101, 8.231249998505111520 ) ) ;
#8185 = CARTESIAN_POINT ( 'NONE',  ( -2.740000000000001545, 8.729000000000002757, 4.313750000000002416 ) ) ;
#8186 = ADVANCED_FACE ( 'NONE', ( #5780 ), #5085, .T. ) ;
#8187 = NEXT_ASSEMBLY_USAGE_OCCURRENCE ( 'NAUO1', ' ', ' ', #516, #6586, $ ) ;
#8188 = NEXT_ASSEMBLY_USAGE_OCCURRENCE ( 'NAUO2', ' ', ' ', #516, #6424, $ ) ;
#8189 = NEXT_ASSEMBLY_USAGE_OCCURRENCE ( 'NAUO3', ' ', ' ', #516, #3856, $ ) ;
#8190 = NEXT_ASSEMBLY_USAGE_OCCURRENCE ( 'NAUO4', ' ', ' ', #516, #1419, $ ) ;
#8191 = NEXT_ASSEMBLY_USAGE_OCCURRENCE ( 'NAUO5', ' ', ' ', #516, #1914, $ ) ;
#8192 = NEXT_ASSEMBLY_USAGE_OCCURRENCE ( 'NAUO6', ' ', ' ', #516, #3521, $ ) ;
#8193 = NEXT_ASSEMBLY_USAGE_OCCURRENCE ( 'NAUO7', ' ', ' ', #516, #2483, $ ) ;
#8194 = NEXT_ASSEMBLY_USAGE_OCCURRENCE ( 'NAUO8', ' ', ' ', #516, #4922, $ ) ;
#8195 = NEXT_ASSEMBLY_USAGE_OCCURRENCE ( 'NAUO9', ' ', ' ', #516, #1622, $ ) ;
#8196 = NEXT_ASSEMBLY_USAGE_OCCURRENCE ( 'NAUO10', ' ', ' ', #2483, #5310, $ ) ;
#8197 = NEXT_ASSEMBLY_USAGE_OCCURRENCE ( 'NAUO11', ' ', ' ', #2483, #1030, $ ) ;
#8198 = NEXT_ASSEMBLY_USAGE_OCCURRENCE ( 'NAUO12', ' ', ' ', #2483, #7978, $ ) ;
#8199 = COLOUR_RGB('Deep Blue', 0.66274510, 0.83137255, 0.94901961);
#8200 = FILL_AREA_STYLE_COLOUR('',#8199);
#8201 = FILL_AREA_STYLE('',(#8200));
#8202 = SURFACE_STYLE_FILL_AREA(#8201);
#8203 = SURFACE_SIDE_STYLE('',(#8202));
#8204 = SURFACE_STYLE_USAGE(.BOTH.,#8203);
#8205 = PRESENTATION_STYLE_ASSIGNMENT((#8204));
#8206 = COLOUR_RGB('Light Blue', 0.31764706, 0.68627451, 0.89019608);
#8207 = FILL_AREA_STYLE_COLOUR('',#8206);
#8208 = FILL_AREA_STYLE('',(#8207));
#8209 = SURFACE_STYLE_FILL_AREA(#8208);
#8210 = SURFACE_SIDE_STYLE('',(#8209));
#8211 = SURFACE_STYLE_USAGE(.BOTH.,#8210);
#8212 = PRESENTATION_STYLE_ASSIGNMENT((#8211));
#8213 = COLOUR_RGB('Sky Blue', 0.40784314, 0.44705882, 0.49803922);
#8214 = FILL_AREA_STYLE_COLOUR('',#8213);
#8215 = FILL_AREA_STYLE('',(#8214));
#8216 = SURFACE_STYLE_FILL_AREA(#8215);
#8217 = SURFACE_SIDE_STYLE('',(#8216));
#8218 = SURFACE_STYLE_USAGE(.BOTH.,#8217);
#8219 = PRESENTATION_STYLE_ASSIGNMENT((#8218));
#8220 = COLOUR_RGB('Slate Gray', 0.72549020, 0.75294118, 0.79215686);
#8221 = FILL_AREA_STYLE_COLOUR('',#8220);
#8222 = FILL_AREA_STYLE('',(#8221));
#8223 = SURFACE_STYLE_FILL_AREA(#8222);
#8224 = SURFACE_SIDE_STYLE('',(#8223));
#8225 = SURFACE_STYLE_USAGE(.BOTH.,#8224);
#8226 = PRESENTATION_STYLE_ASSIGNMENT((#8225));
#8227 = COLOUR_RGB('Light Gray', 0.08235294, 0.09019608, 0.10196078);
#8228 = FILL_AREA_STYLE_COLOUR('',#8227);
#8229 = FILL_AREA_STYLE('',(#8228));
#8230 = SURFACE_STYLE_FILL_AREA(#8229);
#8231 = SURFACE_SIDE_STYLE('',(#8230));
#8232 = SURFACE_STYLE_USAGE(.BOTH.,#8231);
#8233 = PRESENTATION_STYLE_ASSIGNMENT((#8232));
#8234 = COLOUR_RGB('Black', 0.09019608, 0.27058824, 0.51372549);
#8235 = FILL_AREA_STYLE_COLOUR('',#8234);
#8236 = FILL_AREA_STYLE('',(#8235));
#8237 = SURFACE_STYLE_FILL_AREA(#8236);
#8238 = SURFACE_SIDE_STYLE('',(#8237));
#8239 = SURFACE_STYLE_USAGE(.BOTH.,#8238);
#8240 = PRESENTATION_STYLE_ASSIGNMENT((#8239));
#8241 = STYLED_ITEM('',(#8219),#7369);
#8242 = MECHANICAL_DESIGN_GEOMETRIC_PRESENTATION_REPRESENTATION('',(#8241),#3475);
#8243 = STYLED_ITEM('',(#8233),#4597);
#8244 = MECHANICAL_DESIGN_GEOMETRIC_PRESENTATION_REPRESENTATION('',(#8243),#3062);
#8245 = STYLED_ITEM('',(#8226),#7800);
#8246 = MECHANICAL_DESIGN_GEOMETRIC_PRESENTATION_REPRESENTATION('',(#8245),#588);
#8247 = STYLED_ITEM('',(#8233),#7864);
#8248 = MECHANICAL_DESIGN_GEOMETRIC_PRESENTATION_REPRESENTATION('',(#8247),#2017);
#8249 = STYLED_ITEM('',(#8205),#7194);
#8250 = MECHANICAL_DESIGN_GEOMETRIC_PRESENTATION_REPRESENTATION('',(#8249),#1380);
#8251 = STYLED_ITEM('',(#8240),#4616);
#8252 = MECHANICAL_DESIGN_GEOMETRIC_PRESENTATION_REPRESENTATION('',(#8251),#1120);
#8253 = STYLED_ITEM('',(#8212),#7251);
#8254 = MECHANICAL_DESIGN_GEOMETRIC_PRESENTATION_REPRESENTATION('',(#8253),#2811);
#8255 = STYLED_ITEM('',(#8212),#1846);
#8256 = MECHANICAL_DESIGN_GEOMETRIC_PRESENTATION_REPRESENTATION('',(#8255),#1513);
#8257 = STYLED_ITEM('',(#8226),#4468);
#8258 = MECHANICAL_DESIGN_GEOMETRIC_PRESENTATION_REPRESENTATION('',(#8257),#720);
#8259 = STYLED_ITEM('',(#8205),#1772);
#8260 = MECHANICAL_DESIGN_GEOMETRIC_PRESENTATION_REPRESENTATION('',(#8259),#5419);
#8261 = STYLED_ITEM('',(#8219),#2701);
#8262 = MECHANICAL_DESIGN_GEOMETRIC_PRESENTATION_REPRESENTATION('',(#8261),#456);
ENDSEC;
END-ISO-10303-21;
